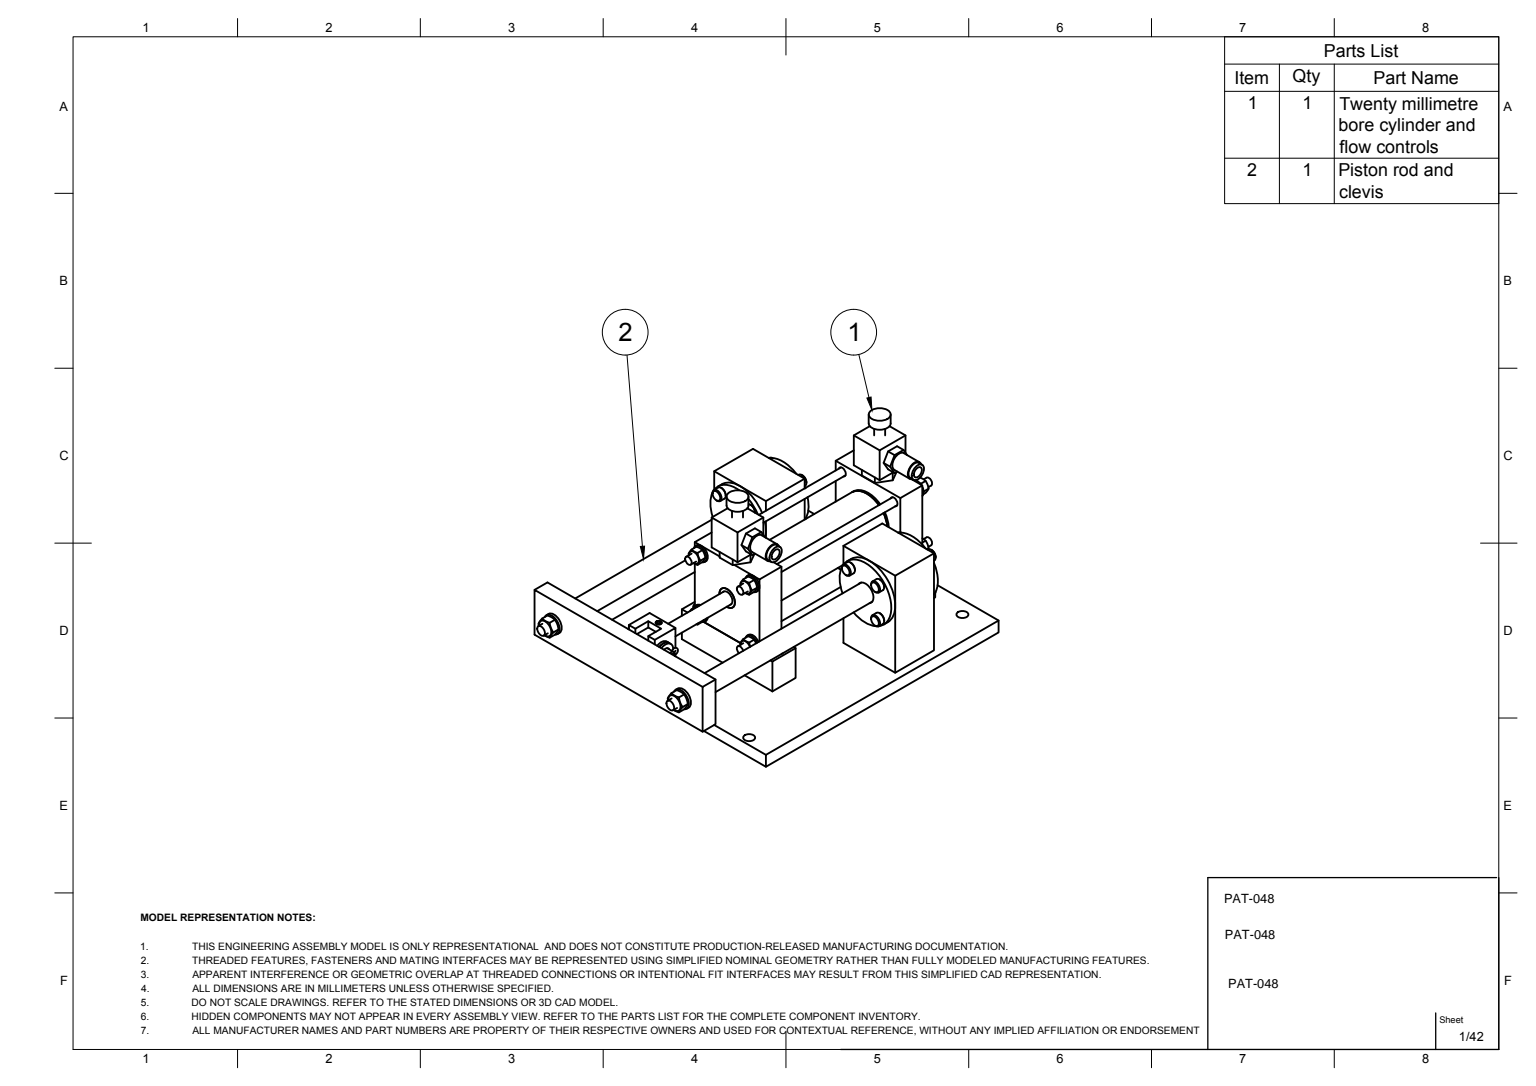
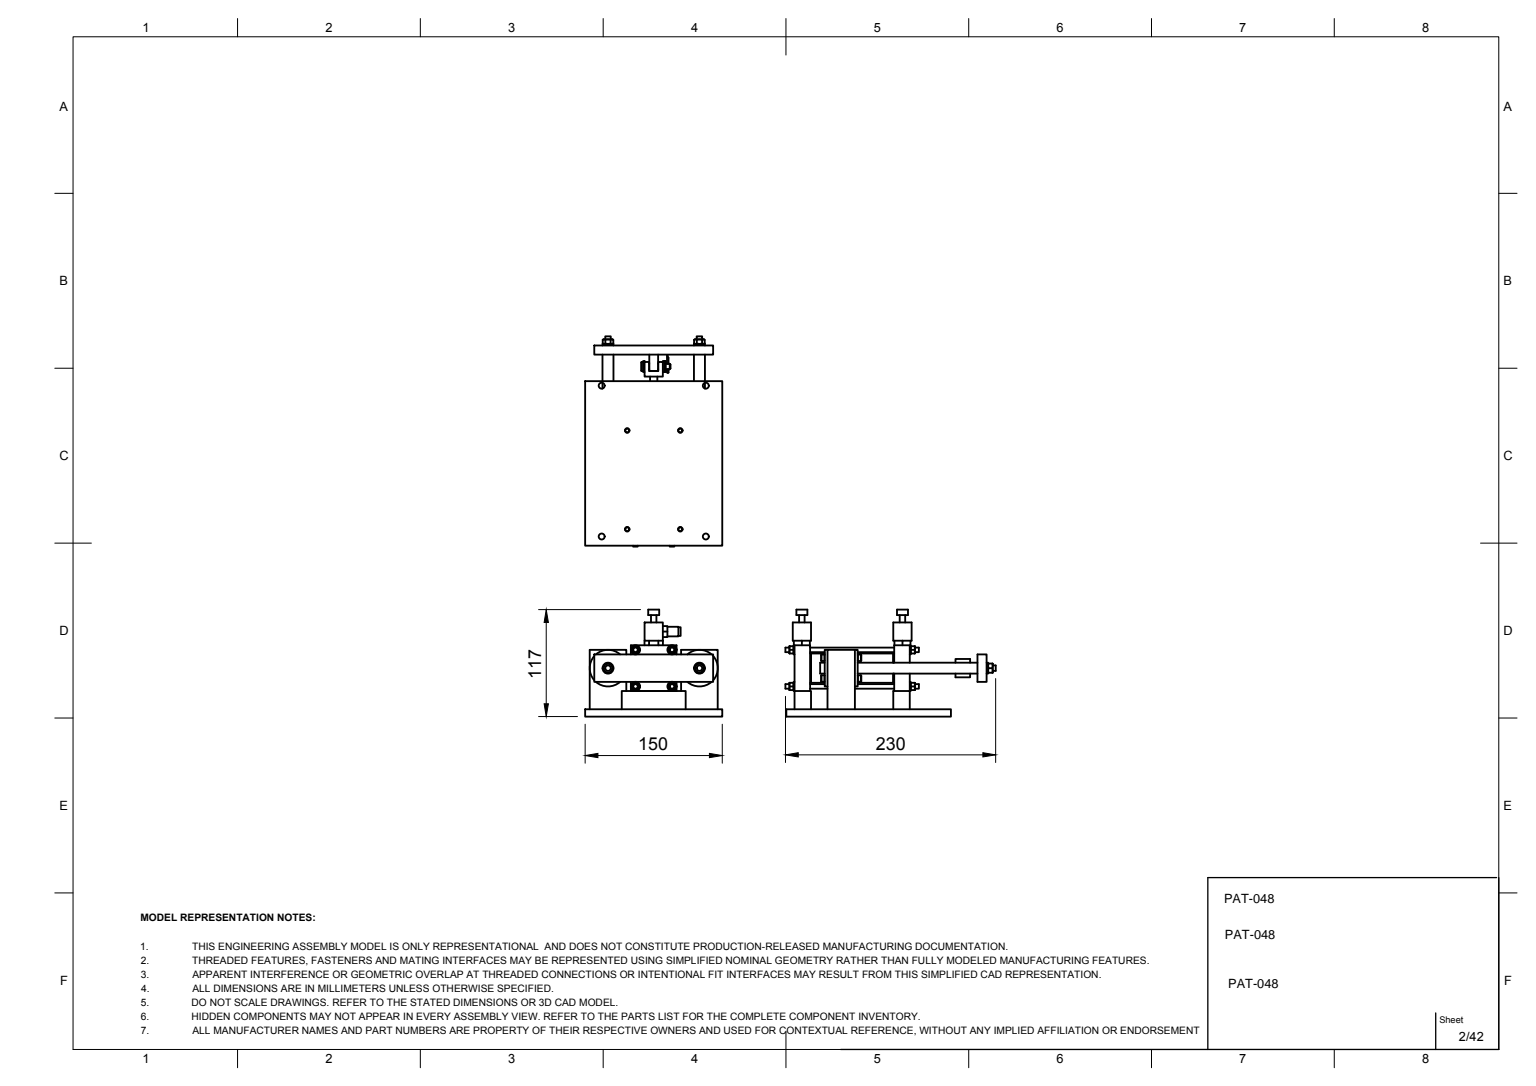
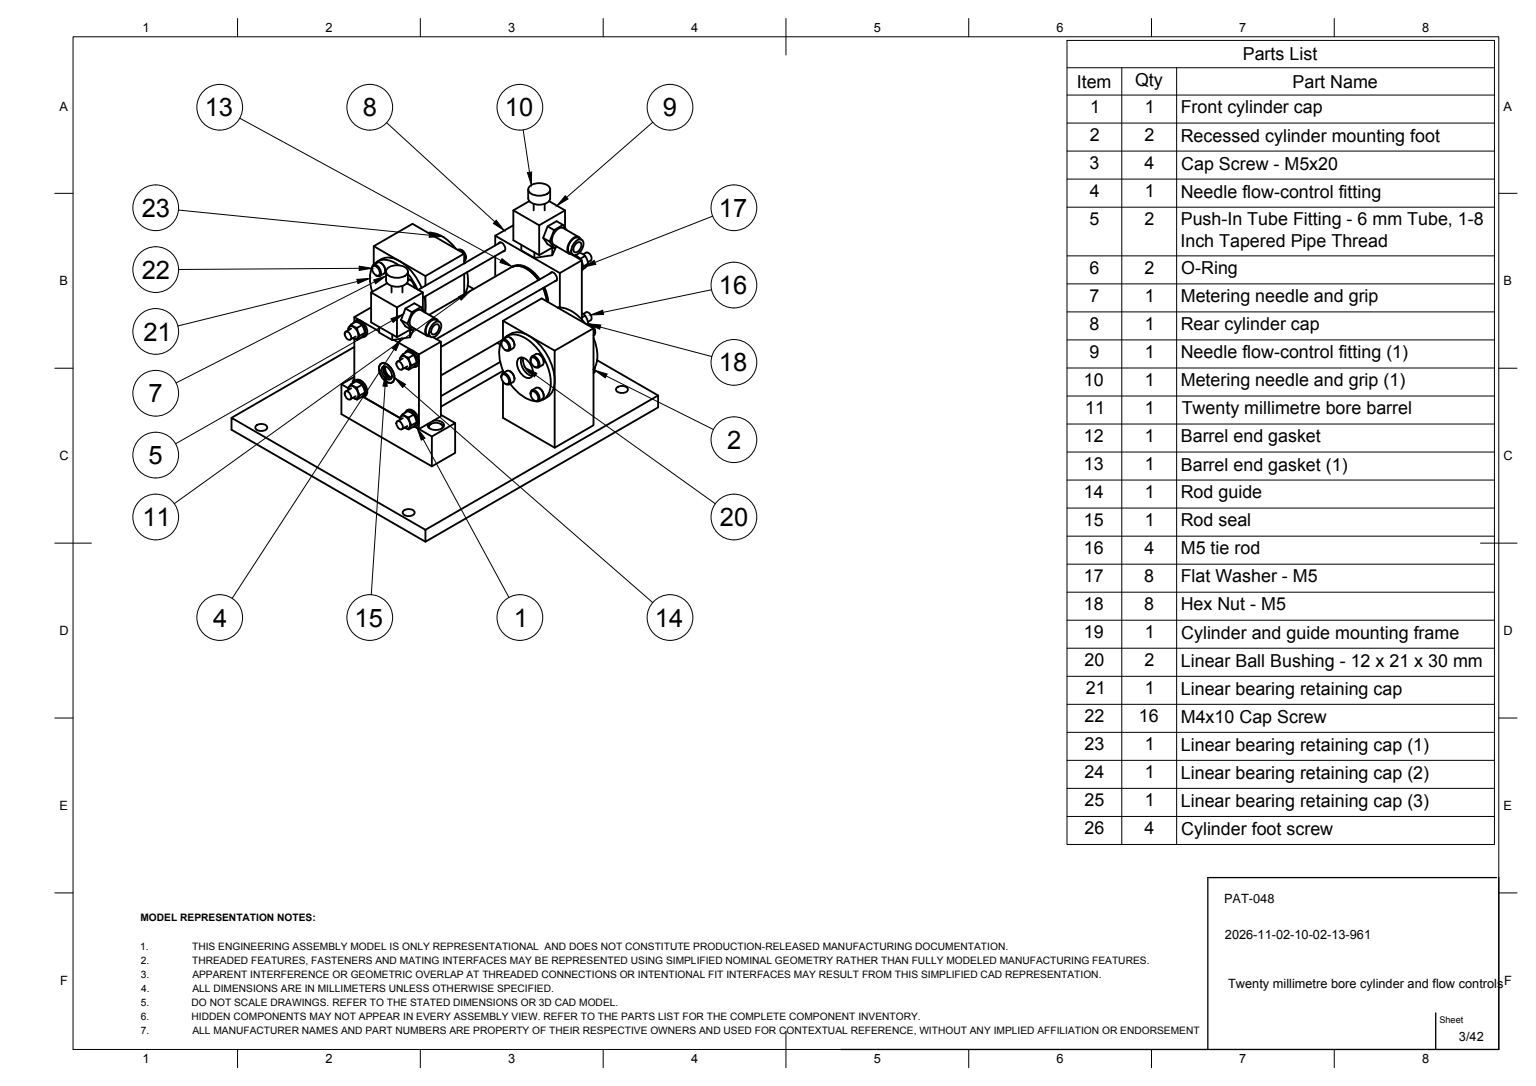
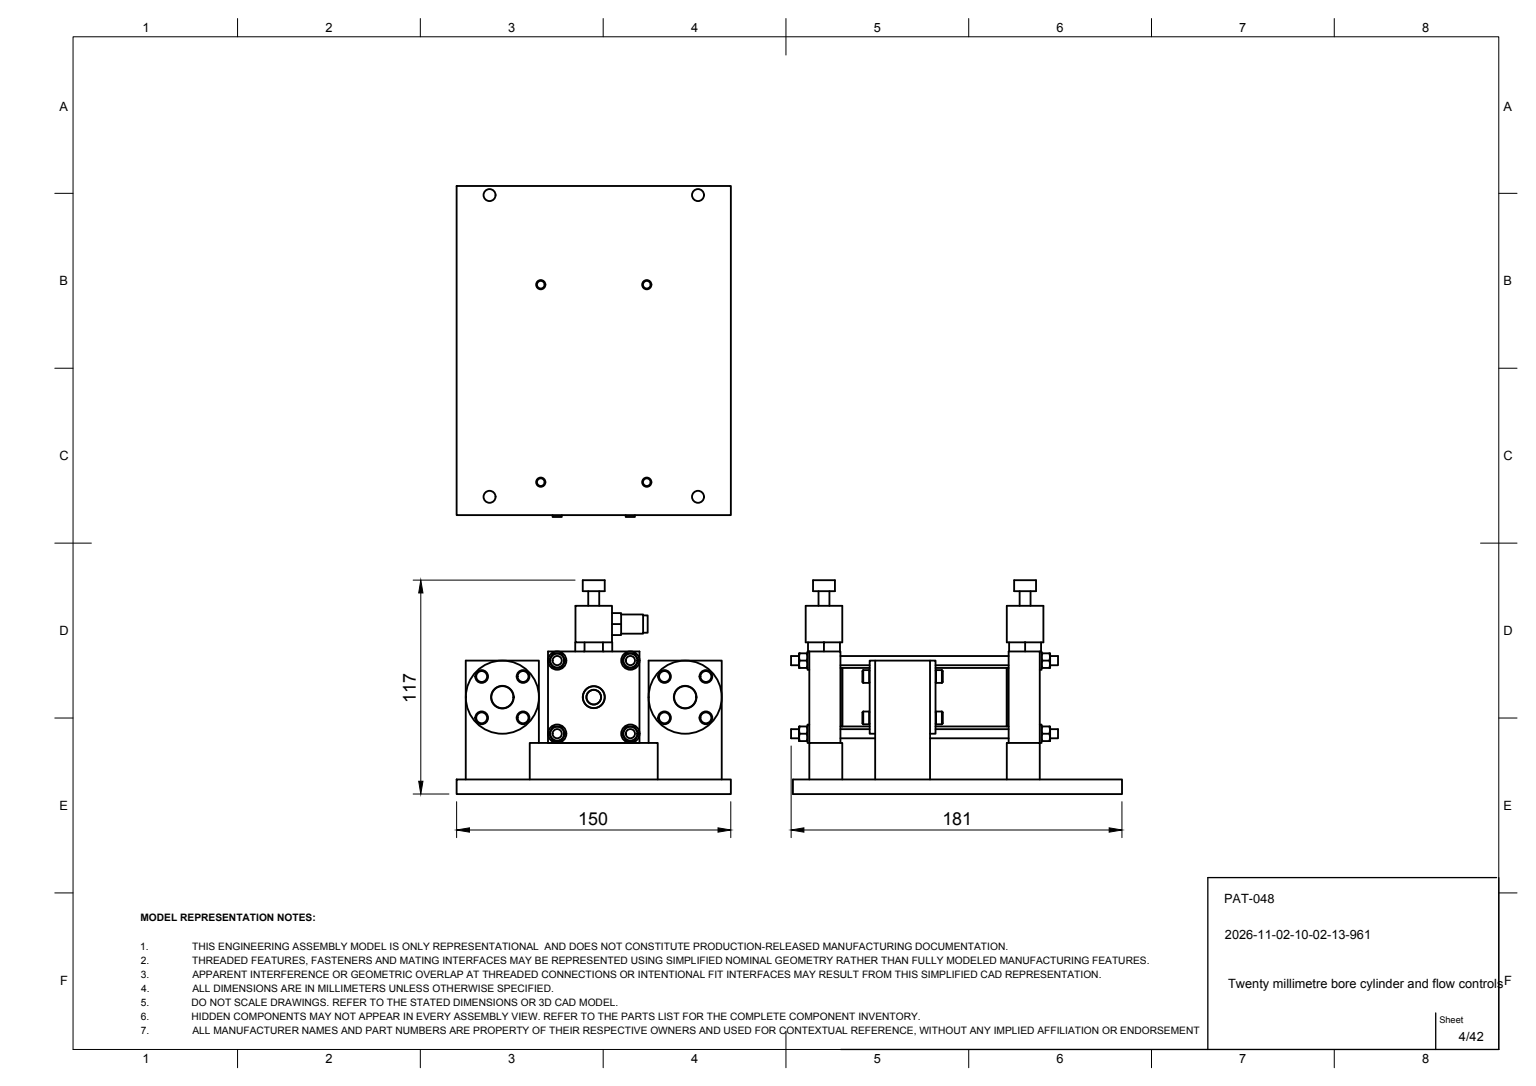
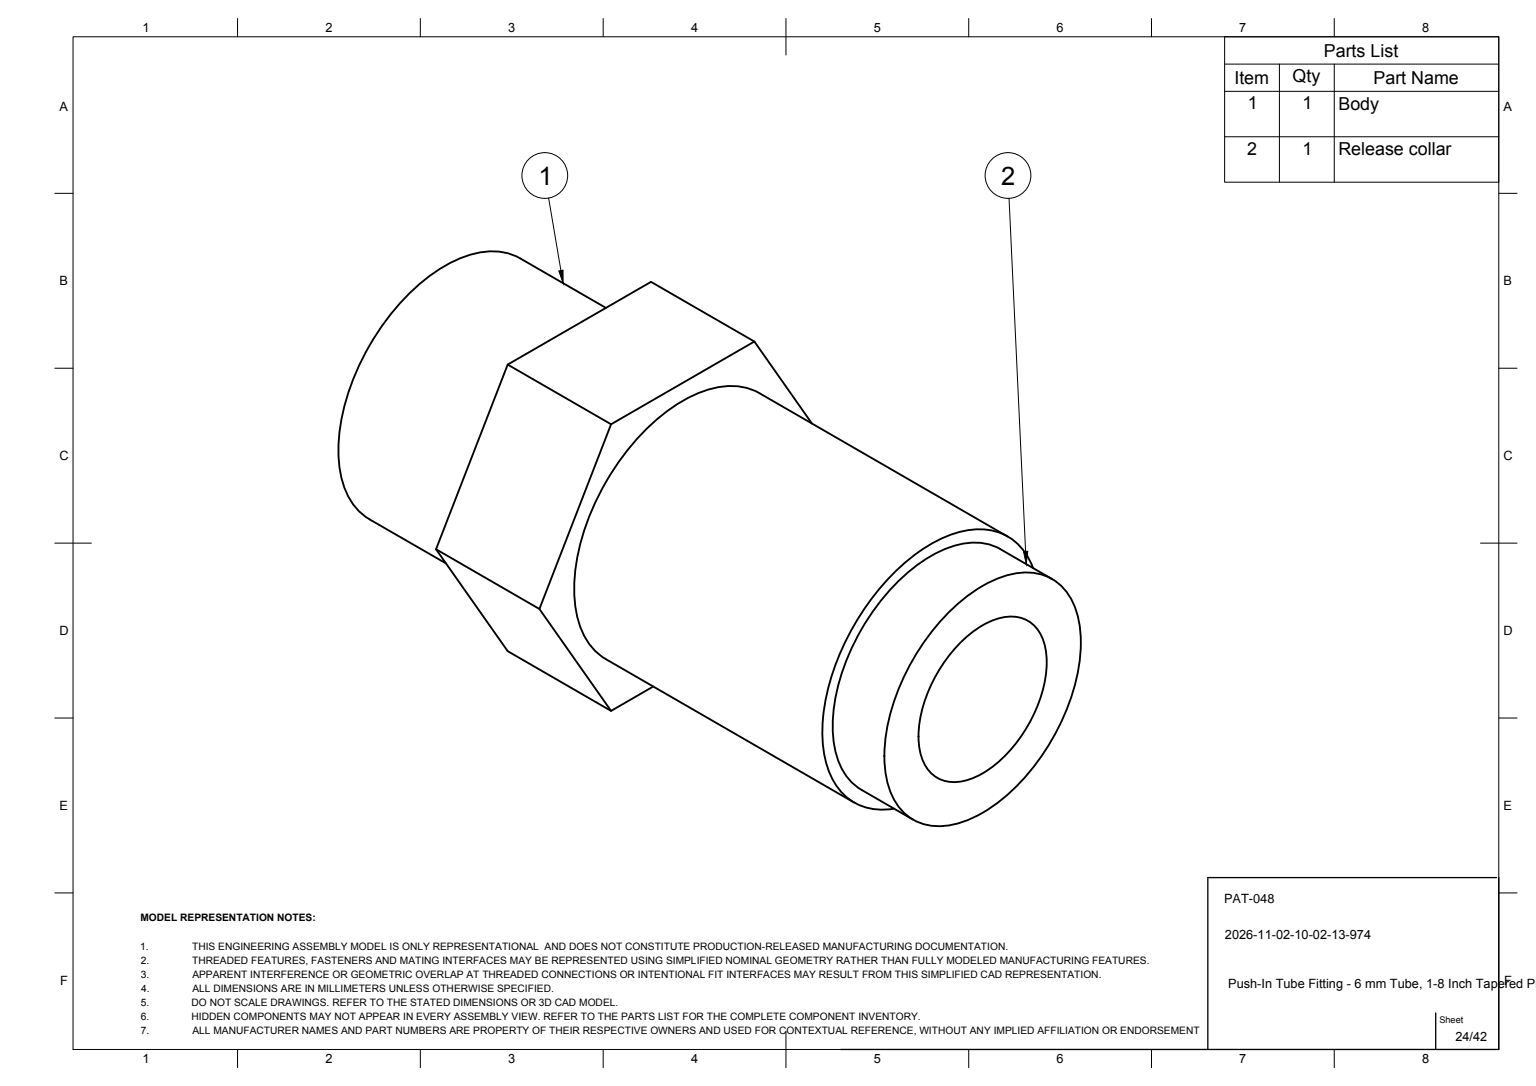
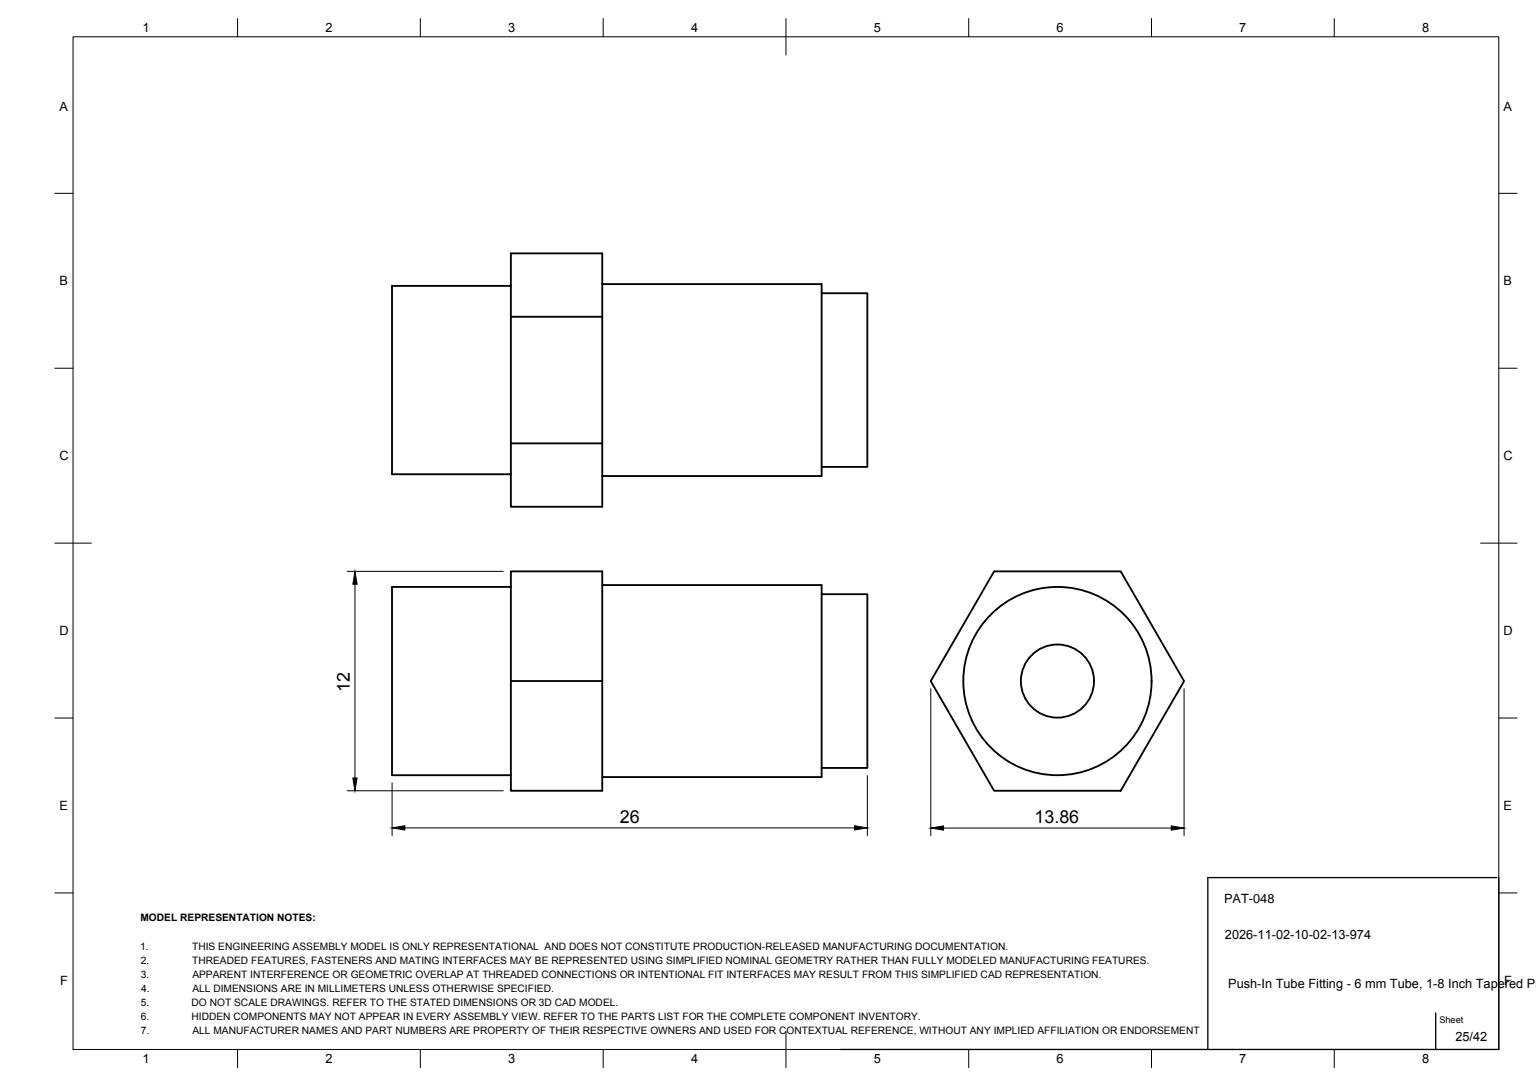
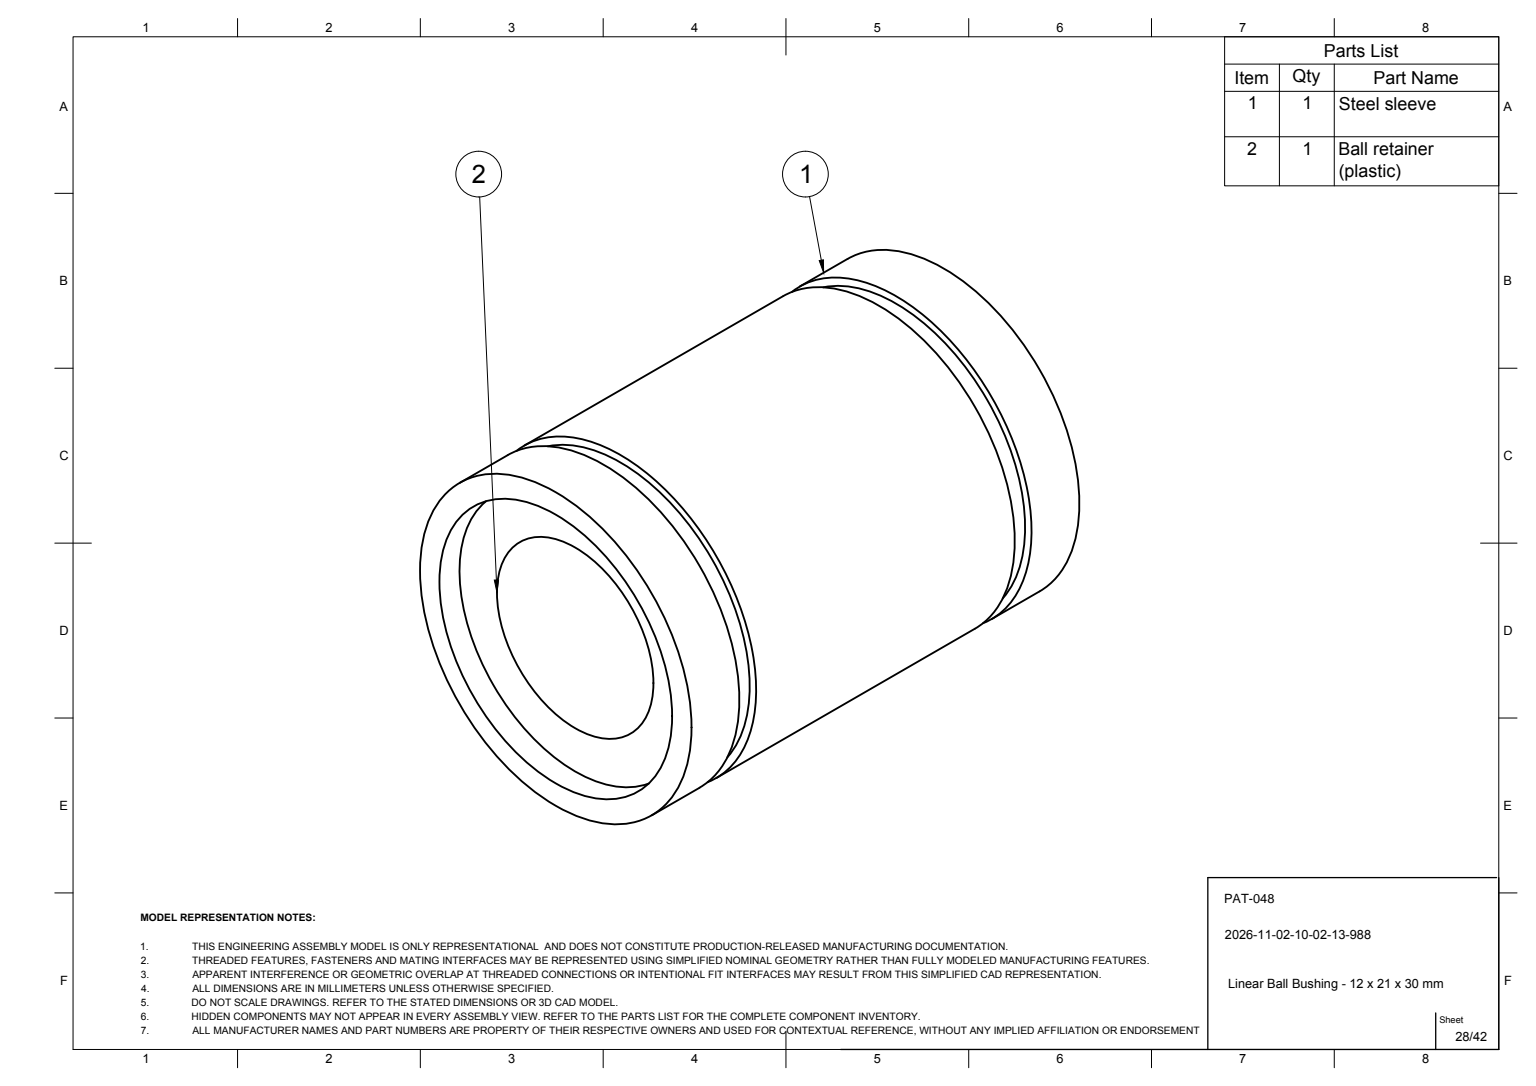
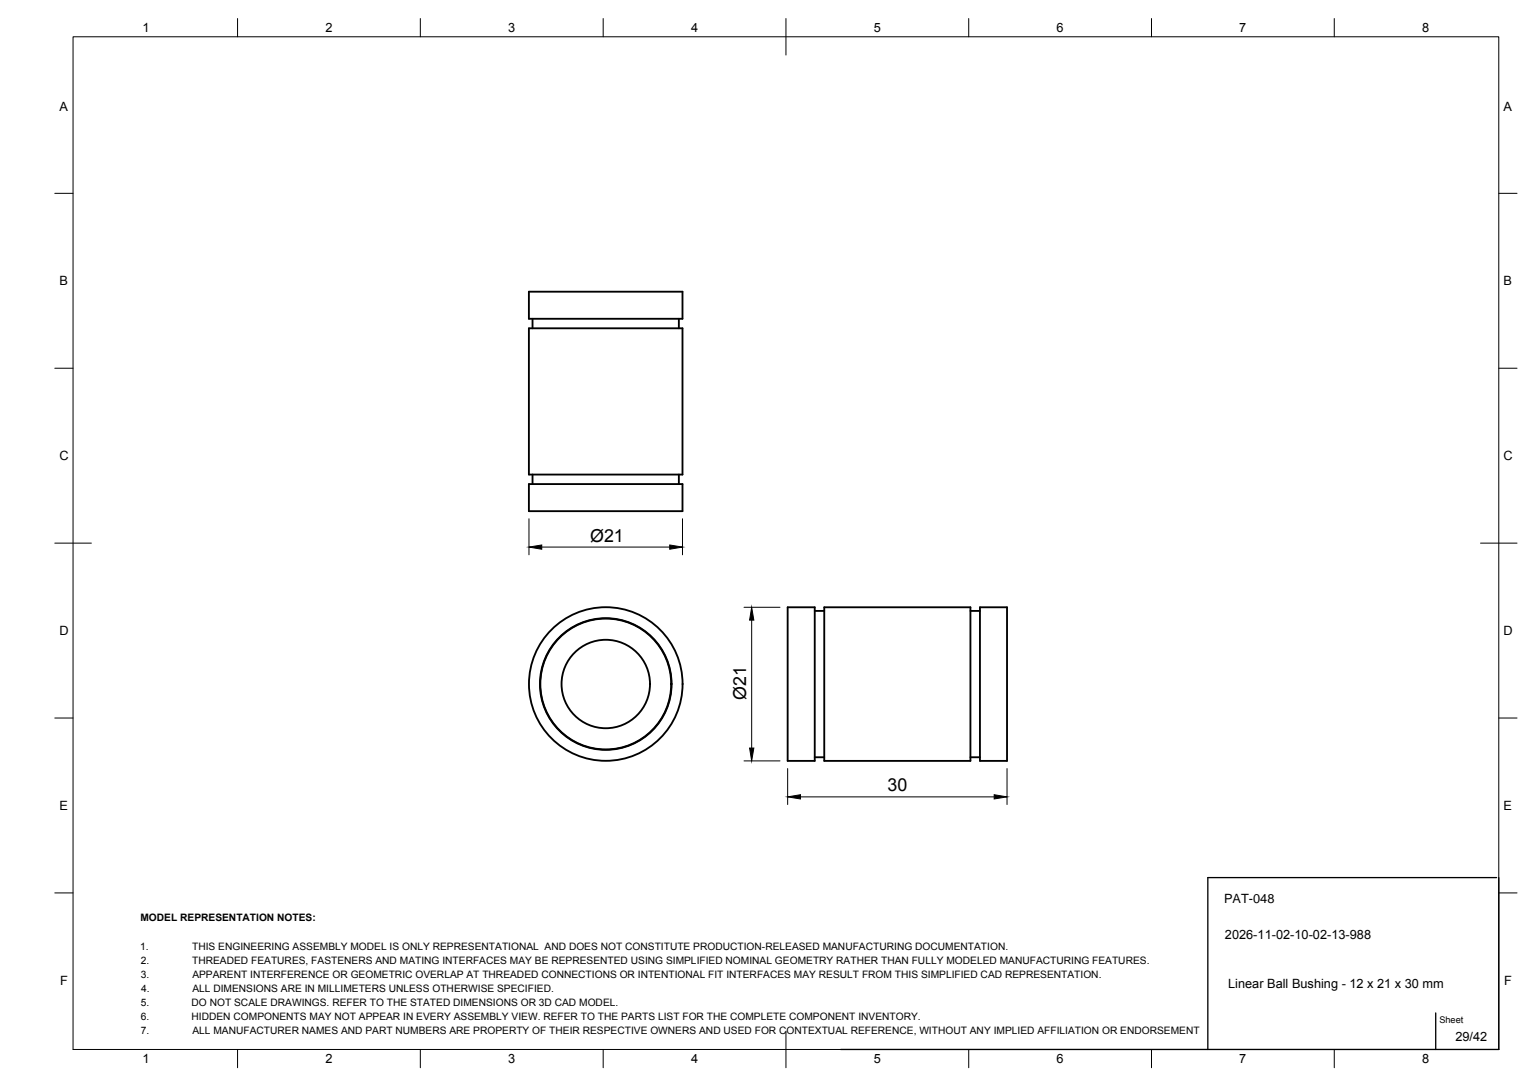
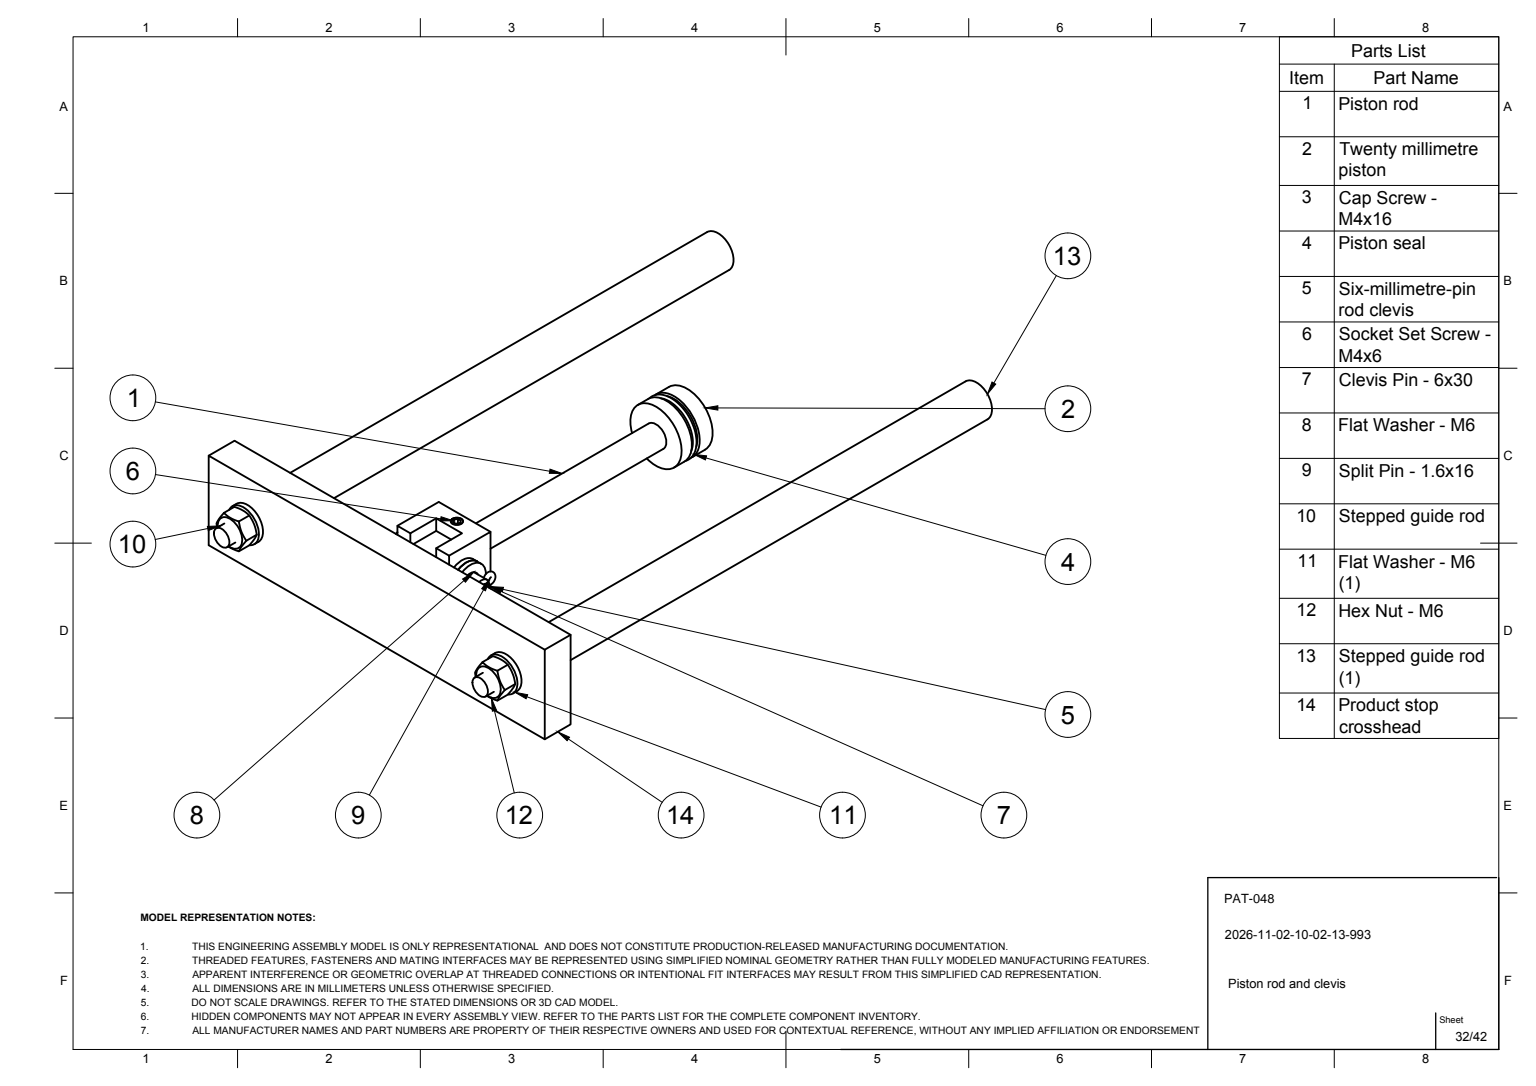
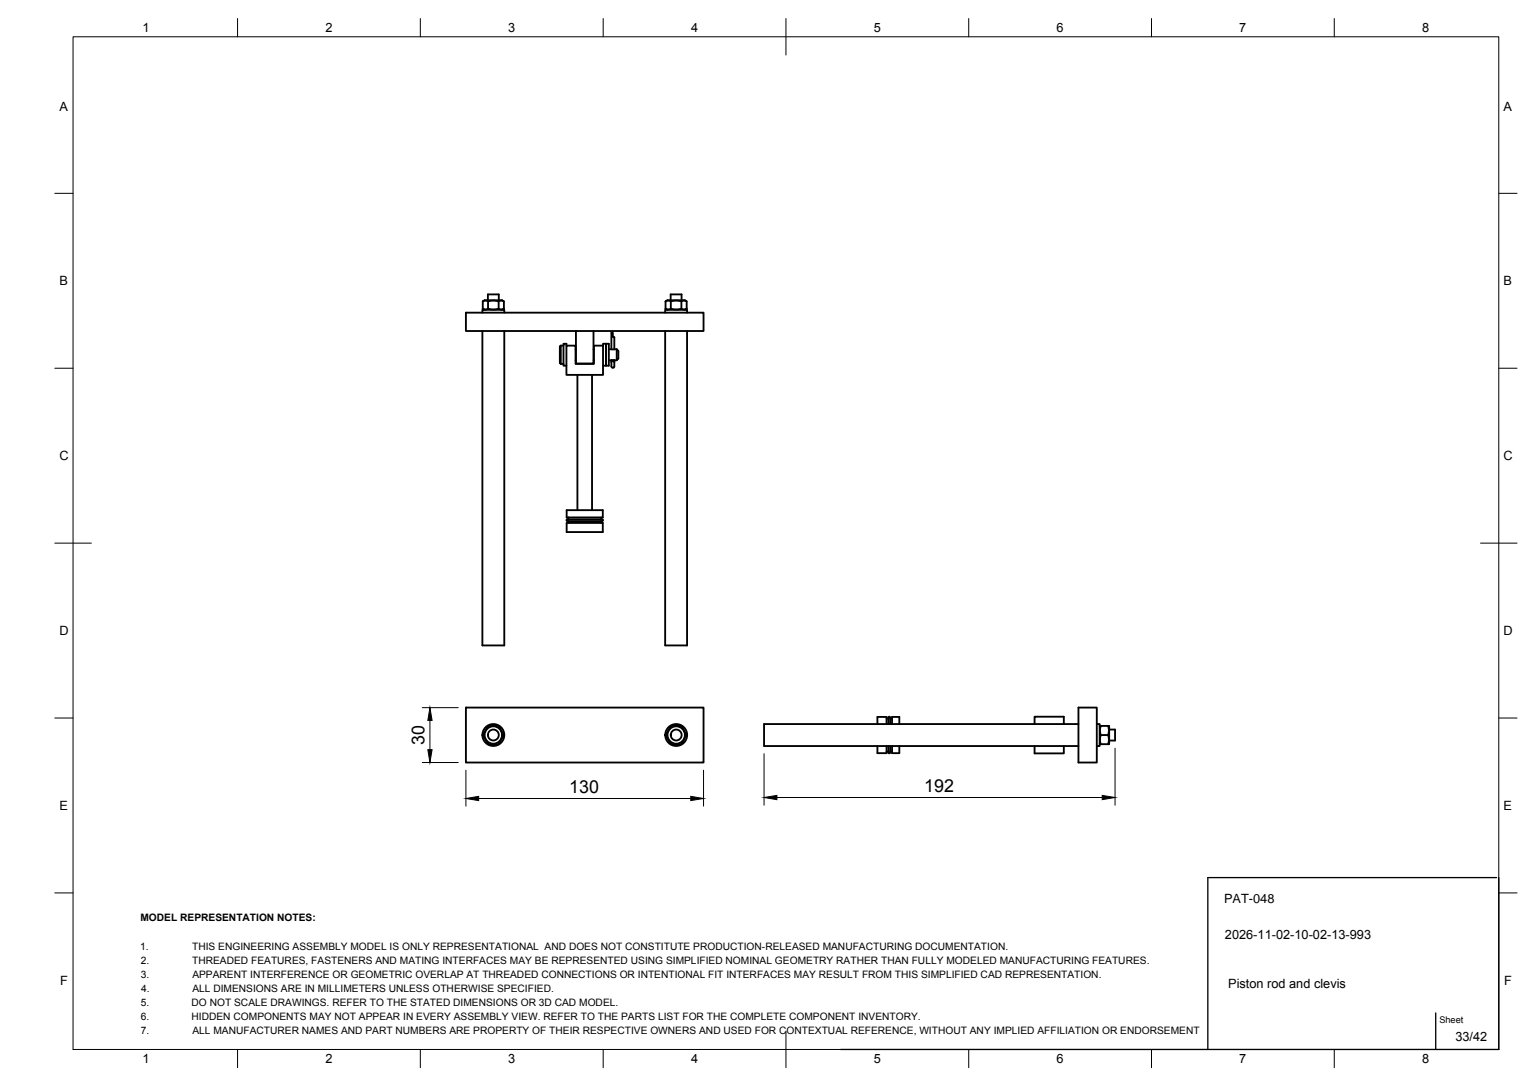
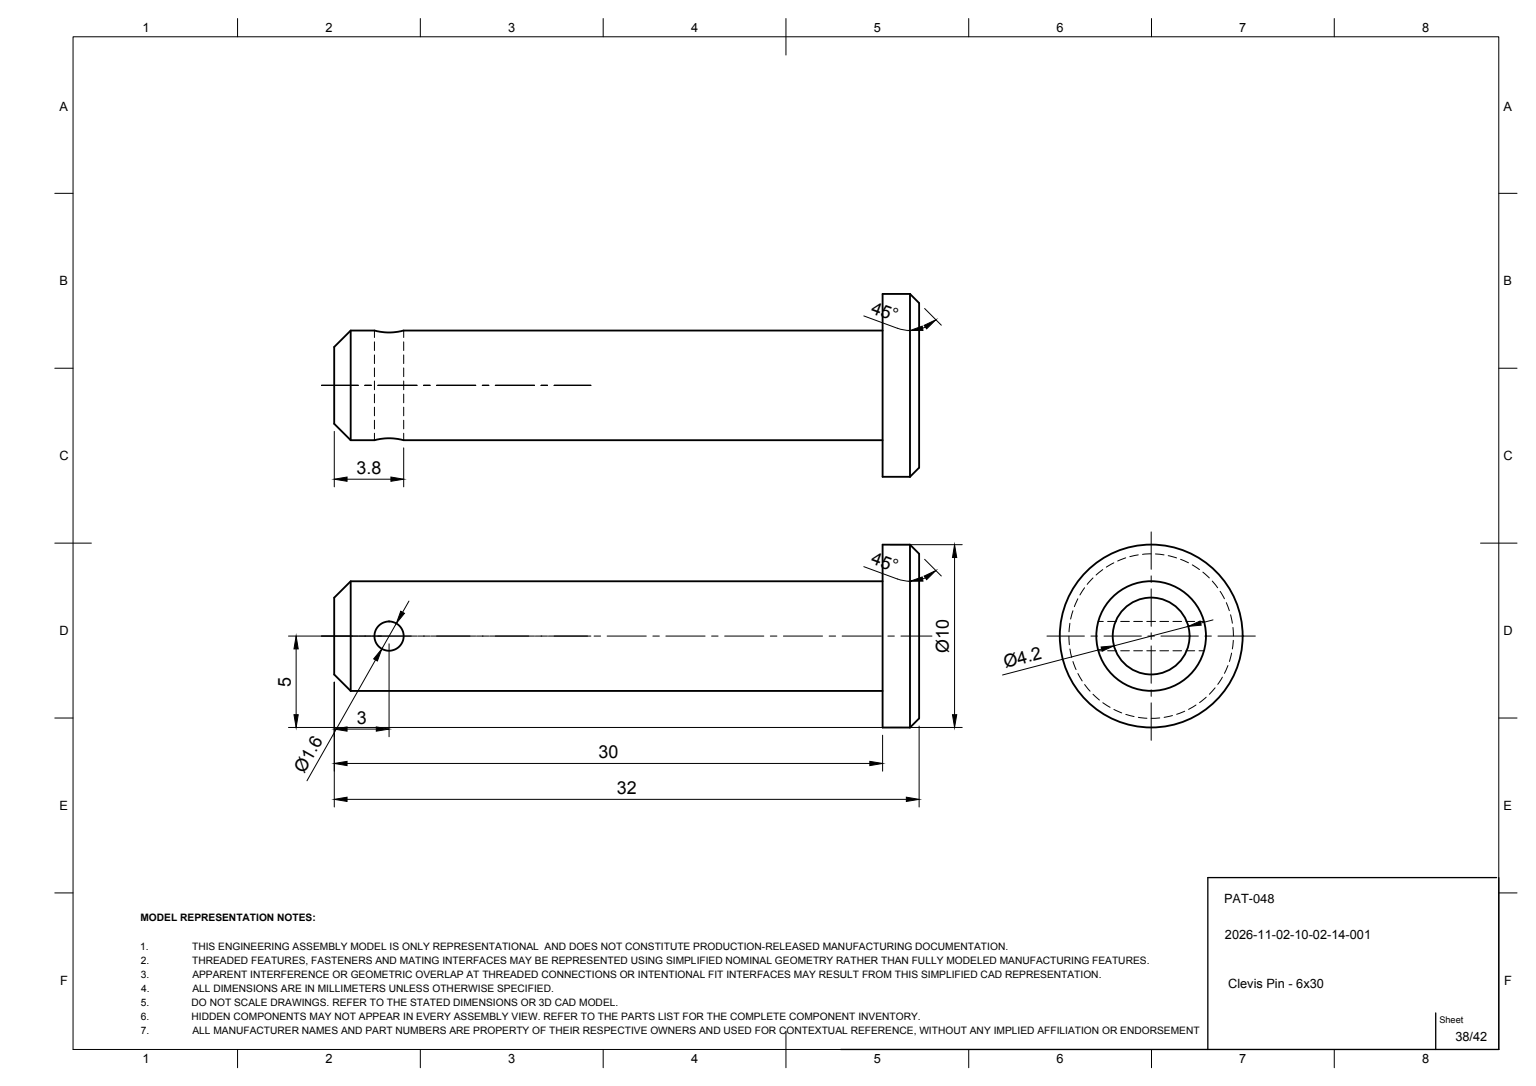
ISO-10303-21;
HEADER;
/* Generated by software containing ST-Developer
 * from STEP Tools, Inc. (www.steptools.com) 
 */

FILE_DESCRIPTION(
/* description */ ('Guided pneumatic stop gate'),
/* implementation_level */ '2;1');

FILE_NAME(
/* name */ 'PAT-048',
/* time_stamp */ '2026-10-27T21:43:45-07:00',
/* author */ (''),
/* organization */ (''),
/* preprocessor_version */ 'ST-DEVELOPER v20.2',
/* originating_system */ 'Autodesk Translation Framework v15.17.0.0',
/* authorisation */ '');

FILE_SCHEMA (('AUTOMOTIVE_DESIGN { 1 0 10303 214 3 1 1 }'));
ENDSEC;

DATA;
#10=MECHANICAL_DESIGN_GEOMETRIC_PRESENTATION_REPRESENTATION('',(#535,#536,
#537,#538,#539,#540,#541,#542,#543,#544,#545,#546,#547,#548,#549,#550,#551,
#552,#553,#554,#555,#556,#557,#558,#559,#560,#561,#562,#563,#564,#565,#566,
#567,#568,#569,#570,#571,#572,#573,#574,#575,#576),#14392);
#11=B_SPLINE_CURVE_WITH_KNOTS('',3,(#13750,#13751,#13752,#13753,#13754,
#13755,#13756,#13757,#13758,#13759),.UNSPECIFIED.,.F.,.F.,(4,2,2,2,4),(0.665271585430998,
0.692803751398643,0.75574615888762,0.818688566376597,0.846220732344242),
 .UNSPECIFIED.);
#12=B_SPLINE_CURVE_WITH_KNOTS('',3,(#13767,#13768,#13769,#13770,#13771,
#13772,#13773,#13774,#13775,#13776),.UNSPECIFIED.,.F.,.F.,(4,2,2,2,4),(0.161440812839251,
0.188972978806896,0.251915386295873,0.31485779378485,0.342389959752495),
 .UNSPECIFIED.);
#13=B_SPLINE_CURVE_WITH_KNOTS('',3,(#13893,#13894,#13895,#13896,#13897,
#13898,#13899,#13900,#13901,#13902),.UNSPECIFIED.,.F.,.F.,(4,2,2,2,4),(0.,
0.0302963256060356,0.0605926512120712,0.090883446720838,0.121174242229605),
 .UNSPECIFIED.);
#14=B_SPLINE_CURVE_WITH_KNOTS('',3,(#13905,#13906,#13907,#13908,#13909,
#13910,#13911,#13912,#13913,#13914,#13915,#13916,#13917,#13918,#13919,#13920,
#13921,#13922,#13923,#13924,#13925,#13926,#13927,#13928,#13929,#13930,#13931,
#13932,#13933,#13934,#13935,#13936,#13937,#13938),.UNSPECIFIED.,.T.,.F.,
(4,2,2,2,2,2,2,2,2,2,2,2,2,2,2,2,4),(0.,0.0302963256060358,0.0605926512120716,
0.0908834467208383,0.121174242229605,0.151465037738372,0.181755833247138,
0.212052158853174,0.24234848445921,0.272644810065246,0.302941135671282,
0.333231931180048,0.363522726688815,0.393813522197582,0.424104317706349,
0.454400643312384,0.48469696891842),.UNSPECIFIED.);
#15=B_SPLINE_CURVE_WITH_KNOTS('',3,(#13940,#13941,#13942,#13943,#13944,
#13945,#13946,#13947,#13948,#13949),.UNSPECIFIED.,.F.,.F.,(4,2,2,2,4),(0.363522726688815,
0.393813522197581,0.424104317706348,0.454400643312384,0.48469696891842),
 .UNSPECIFIED.);
#16=B_SPLINE_CURVE_WITH_KNOTS('',3,(#13950,#13951,#13952,#13953,#13954,
#13955,#13956,#13957,#13958,#13959,#13960,#13961,#13962,#13963,#13964,#13965,
#13966,#13967),.UNSPECIFIED.,.F.,.F.,(4,2,2,2,2,2,2,2,4),(0.121174242229605,
0.151465037738371,0.181755833247138,0.212052158853174,0.24234848445921,
0.272644810065246,0.302941135671281,0.333231931180048,0.363522726688815),
 .UNSPECIFIED.);
#17=B_SPLINE_CURVE_WITH_KNOTS('',3,(#14014,#14015,#14016,#14017,#14018,
#14019,#14020,#14021,#14022,#14023,#14024,#14025,#14026,#14027,#14028,#14029,
#14030,#14031,#14032,#14033,#14034,#14035,#14036,#14037,#14038,#14039),
 .UNSPECIFIED.,.F.,.F.,(4,2,2,2,2,2,2,2,2,2,2,2,4),(-0.00054581412719389,
0.,0.0281583564005144,0.0618496465371181,0.0905865724114538,0.120694112793616,
0.144966158459363,0.16923820412511,0.199345744507272,0.228082670381608,
0.261773960518212,0.289932316918681,0.290478131045882),.UNSPECIFIED.);
#18=B_SPLINE_CURVE_WITH_KNOTS('',3,(#14040,#14041,#14042,#14043,#14044,
#14045,#14046,#14047,#14048,#14049,#14050,#14051,#14052,#14053,#14054,#14055,
#14056,#14057,#14058,#14059,#14060,#14061,#14062,#14063,#14064,#14065),
 .UNSPECIFIED.,.F.,.F.,(4,2,2,2,2,2,2,2,2,2,2,2,4),(-0.000545814127196571,
0.,0.0281583564006391,0.0618496465374156,0.0905865724118984,0.120694112794215,
0.144966158460086,0.169238204125958,0.199345744508275,0.228082670382758,
0.261773960519534,0.289932316920171,0.29047813104737),.UNSPECIFIED.);
#19=(
BOUNDED_CURVE()
B_SPLINE_CURVE(2,(#12867,#12868,#12869),.UNSPECIFIED.,.F.,.F.)
B_SPLINE_CURVE_WITH_KNOTS((3,3),(0.140651836354967,0.670383167684795),
 .UNSPECIFIED.)
CURVE()
GEOMETRIC_REPRESENTATION_ITEM()
RATIONAL_B_SPLINE_CURVE((1.11602540378444,1.28867513459481,1.11602540378444))
REPRESENTATION_ITEM('')
);
#20=(
BOUNDED_CURVE()
B_SPLINE_CURVE(2,(#12871,#12872,#12873),.UNSPECIFIED.,.F.,.F.)
B_SPLINE_CURVE_WITH_KNOTS((3,3),(0.140651836354967,0.670383167684795),
 .UNSPECIFIED.)
CURVE()
GEOMETRIC_REPRESENTATION_ITEM()
RATIONAL_B_SPLINE_CURVE((1.11602540378444,1.28867513459481,1.11602540378444))
REPRESENTATION_ITEM('')
);
#21=(
BOUNDED_CURVE()
B_SPLINE_CURVE(2,(#12878,#12879,#12880),.UNSPECIFIED.,.F.,.F.)
B_SPLINE_CURVE_WITH_KNOTS((3,3),(0.140651836354967,0.670383167684795),
 .UNSPECIFIED.)
CURVE()
GEOMETRIC_REPRESENTATION_ITEM()
RATIONAL_B_SPLINE_CURVE((1.11602540378444,1.28867513459481,1.11602540378444))
REPRESENTATION_ITEM('')
);
#22=(
BOUNDED_CURVE()
B_SPLINE_CURVE(2,(#12882,#12883,#12884),.UNSPECIFIED.,.F.,.F.)
B_SPLINE_CURVE_WITH_KNOTS((3,3),(0.140651836354967,0.670383167684795),
 .UNSPECIFIED.)
CURVE()
GEOMETRIC_REPRESENTATION_ITEM()
RATIONAL_B_SPLINE_CURVE((1.11602540378444,1.28867513459481,1.11602540378444))
REPRESENTATION_ITEM('')
);
#23=(
BOUNDED_CURVE()
B_SPLINE_CURVE(2,(#12886,#12887,#12888),.UNSPECIFIED.,.F.,.F.)
B_SPLINE_CURVE_WITH_KNOTS((3,3),(0.140651836354967,0.670383167684795),
 .UNSPECIFIED.)
CURVE()
GEOMETRIC_REPRESENTATION_ITEM()
RATIONAL_B_SPLINE_CURVE((1.11602540378444,1.28867513459481,1.11602540378444))
REPRESENTATION_ITEM('')
);
#24=(
BOUNDED_CURVE()
B_SPLINE_CURVE(2,(#12889,#12890,#12891),.UNSPECIFIED.,.F.,.F.)
B_SPLINE_CURVE_WITH_KNOTS((3,3),(0.140651836354967,0.670383167684795),
 .UNSPECIFIED.)
CURVE()
GEOMETRIC_REPRESENTATION_ITEM()
RATIONAL_B_SPLINE_CURVE((1.11602540378444,1.28867513459481,1.11602540378444))
REPRESENTATION_ITEM('')
);
#25=(
BOUNDED_CURVE()
B_SPLINE_CURVE(2,(#12898,#12899,#12900),.UNSPECIFIED.,.F.,.F.)
B_SPLINE_CURVE_WITH_KNOTS((3,3),(0.140651836354967,0.670383167684795),
 .UNSPECIFIED.)
CURVE()
GEOMETRIC_REPRESENTATION_ITEM()
RATIONAL_B_SPLINE_CURVE((1.11602540378444,1.28867513459481,1.11602540378444))
REPRESENTATION_ITEM('')
);
#26=(
BOUNDED_CURVE()
B_SPLINE_CURVE(2,(#12902,#12903,#12904),.UNSPECIFIED.,.F.,.F.)
B_SPLINE_CURVE_WITH_KNOTS((3,3),(0.140651836354967,0.670383167684796),
 .UNSPECIFIED.)
CURVE()
GEOMETRIC_REPRESENTATION_ITEM()
RATIONAL_B_SPLINE_CURVE((1.11602540378444,1.28867513459481,1.11602540378444))
REPRESENTATION_ITEM('')
);
#27=(
BOUNDED_CURVE()
B_SPLINE_CURVE(2,(#12906,#12907,#12908),.UNSPECIFIED.,.F.,.F.)
B_SPLINE_CURVE_WITH_KNOTS((3,3),(0.140651836354967,0.670383167684795),
 .UNSPECIFIED.)
CURVE()
GEOMETRIC_REPRESENTATION_ITEM()
RATIONAL_B_SPLINE_CURVE((1.11602540378444,1.28867513459481,1.11602540378444))
REPRESENTATION_ITEM('')
);
#28=(
BOUNDED_CURVE()
B_SPLINE_CURVE(2,(#12910,#12911,#12912),.UNSPECIFIED.,.F.,.F.)
B_SPLINE_CURVE_WITH_KNOTS((3,3),(0.140651836354967,0.670383167684795),
 .UNSPECIFIED.)
CURVE()
GEOMETRIC_REPRESENTATION_ITEM()
RATIONAL_B_SPLINE_CURVE((1.11602540378444,1.28867513459482,1.11602540378444))
REPRESENTATION_ITEM('')
);
#29=(
BOUNDED_CURVE()
B_SPLINE_CURVE(2,(#12914,#12915,#12916),.UNSPECIFIED.,.F.,.F.)
B_SPLINE_CURVE_WITH_KNOTS((3,3),(0.140651836354967,0.670383167684795),
 .UNSPECIFIED.)
CURVE()
GEOMETRIC_REPRESENTATION_ITEM()
RATIONAL_B_SPLINE_CURVE((1.11602540378444,1.28867513459481,1.11602540378444))
REPRESENTATION_ITEM('')
);
#30=(
BOUNDED_CURVE()
B_SPLINE_CURVE(2,(#12917,#12918,#12919),.UNSPECIFIED.,.F.,.F.)
B_SPLINE_CURVE_WITH_KNOTS((3,3),(0.140651836354967,0.670383167684795),
 .UNSPECIFIED.)
CURVE()
GEOMETRIC_REPRESENTATION_ITEM()
RATIONAL_B_SPLINE_CURVE((1.11602540378444,1.28867513459481,1.11602540378444))
REPRESENTATION_ITEM('')
);
#31=(
BOUNDED_CURVE()
B_SPLINE_CURVE(2,(#14204,#14205,#14206),.UNSPECIFIED.,.F.,.F.)
B_SPLINE_CURVE_WITH_KNOTS((3,3),(0.144988513094728,0.791574906712449),
 .UNSPECIFIED.)
CURVE()
GEOMETRIC_REPRESENTATION_ITEM()
RATIONAL_B_SPLINE_CURVE((1.09282032302755,1.26188021535082,1.09282032302931))
REPRESENTATION_ITEM('')
);
#32=(
BOUNDED_CURVE()
B_SPLINE_CURVE(2,(#14208,#14209,#14210),.UNSPECIFIED.,.F.,.F.)
B_SPLINE_CURVE_WITH_KNOTS((3,3),(0.144988513094728,0.791574906712449),
 .UNSPECIFIED.)
CURVE()
GEOMETRIC_REPRESENTATION_ITEM()
RATIONAL_B_SPLINE_CURVE((1.09282032302755,1.26188021535082,1.09282032302931))
REPRESENTATION_ITEM('')
);
#33=(
BOUNDED_CURVE()
B_SPLINE_CURVE(2,(#14215,#14216,#14217),.UNSPECIFIED.,.F.,.F.)
B_SPLINE_CURVE_WITH_KNOTS((3,3),(0.144988513094728,0.791574906712449),
 .UNSPECIFIED.)
CURVE()
GEOMETRIC_REPRESENTATION_ITEM()
RATIONAL_B_SPLINE_CURVE((1.09282032302755,1.26188021535082,1.09282032302931))
REPRESENTATION_ITEM('')
);
#34=(
BOUNDED_CURVE()
B_SPLINE_CURVE(2,(#14219,#14220,#14221),.UNSPECIFIED.,.F.,.F.)
B_SPLINE_CURVE_WITH_KNOTS((3,3),(0.144988513094728,0.791574906712449),
 .UNSPECIFIED.)
CURVE()
GEOMETRIC_REPRESENTATION_ITEM()
RATIONAL_B_SPLINE_CURVE((1.09282032302755,1.26188021535082,1.09282032302931))
REPRESENTATION_ITEM('')
);
#35=(
BOUNDED_CURVE()
B_SPLINE_CURVE(2,(#14223,#14224,#14225),.UNSPECIFIED.,.F.,.F.)
B_SPLINE_CURVE_WITH_KNOTS((3,3),(0.144988513094728,0.791574906712449),
 .UNSPECIFIED.)
CURVE()
GEOMETRIC_REPRESENTATION_ITEM()
RATIONAL_B_SPLINE_CURVE((1.09282032302755,1.26188021535082,1.09282032302931))
REPRESENTATION_ITEM('')
);
#36=(
BOUNDED_CURVE()
B_SPLINE_CURVE(2,(#14226,#14227,#14228),.UNSPECIFIED.,.F.,.F.)
B_SPLINE_CURVE_WITH_KNOTS((3,3),(0.144988513094728,0.791574906712449),
 .UNSPECIFIED.)
CURVE()
GEOMETRIC_REPRESENTATION_ITEM()
RATIONAL_B_SPLINE_CURVE((1.09282032302755,1.26188021535082,1.09282032302931))
REPRESENTATION_ITEM('')
);
#37=(
BOUNDED_CURVE()
B_SPLINE_CURVE(2,(#14235,#14236,#14237),.UNSPECIFIED.,.F.,.F.)
B_SPLINE_CURVE_WITH_KNOTS((3,3),(0.144988513094728,0.791574906712449),
 .UNSPECIFIED.)
CURVE()
GEOMETRIC_REPRESENTATION_ITEM()
RATIONAL_B_SPLINE_CURVE((1.09282032302755,1.26188021535082,1.09282032302931))
REPRESENTATION_ITEM('')
);
#38=(
BOUNDED_CURVE()
B_SPLINE_CURVE(2,(#14239,#14240,#14241),.UNSPECIFIED.,.F.,.F.)
B_SPLINE_CURVE_WITH_KNOTS((3,3),(0.144988513094727,0.791574906712449),
 .UNSPECIFIED.)
CURVE()
GEOMETRIC_REPRESENTATION_ITEM()
RATIONAL_B_SPLINE_CURVE((1.09282032302755,1.26188021535082,1.09282032302931))
REPRESENTATION_ITEM('')
);
#39=(
BOUNDED_CURVE()
B_SPLINE_CURVE(2,(#14243,#14244,#14245),.UNSPECIFIED.,.F.,.F.)
B_SPLINE_CURVE_WITH_KNOTS((3,3),(0.144988513094728,0.791574906712449),
 .UNSPECIFIED.)
CURVE()
GEOMETRIC_REPRESENTATION_ITEM()
RATIONAL_B_SPLINE_CURVE((1.09282032302755,1.26188021535082,1.09282032302931))
REPRESENTATION_ITEM('')
);
#40=(
BOUNDED_CURVE()
B_SPLINE_CURVE(2,(#14247,#14248,#14249),.UNSPECIFIED.,.F.,.F.)
B_SPLINE_CURVE_WITH_KNOTS((3,3),(0.144988513094728,0.791574906712449),
 .UNSPECIFIED.)
CURVE()
GEOMETRIC_REPRESENTATION_ITEM()
RATIONAL_B_SPLINE_CURVE((1.09282032302755,1.26188021535082,1.09282032302931))
REPRESENTATION_ITEM('')
);
#41=(
BOUNDED_CURVE()
B_SPLINE_CURVE(2,(#14251,#14252,#14253),.UNSPECIFIED.,.F.,.F.)
B_SPLINE_CURVE_WITH_KNOTS((3,3),(0.144988513094728,0.791574906712449),
 .UNSPECIFIED.)
CURVE()
GEOMETRIC_REPRESENTATION_ITEM()
RATIONAL_B_SPLINE_CURVE((1.09282032302755,1.26188021535082,1.09282032302931))
REPRESENTATION_ITEM('')
);
#42=(
BOUNDED_CURVE()
B_SPLINE_CURVE(2,(#14254,#14255,#14256),.UNSPECIFIED.,.F.,.F.)
B_SPLINE_CURVE_WITH_KNOTS((3,3),(0.144988513094727,0.791574906712449),
 .UNSPECIFIED.)
CURVE()
GEOMETRIC_REPRESENTATION_ITEM()
RATIONAL_B_SPLINE_CURVE((1.09282032302755,1.26188021535082,1.09282032302931))
REPRESENTATION_ITEM('')
);
#43=TOROIDAL_SURFACE('',#8768,0.3925,0.089);
#44=TOROIDAL_SURFACE('',#8789,0.45,0.05);
#45=TOROIDAL_SURFACE('',#9177,0.95,0.05);
#46=TOROIDAL_SURFACE('',#9285,0.12,0.08);
#47=ITEM_DEFINED_TRANSFORMATION($,$,#8724,#8765);
#48=ITEM_DEFINED_TRANSFORMATION($,$,#8752,#8766);
#49=ITEM_DEFINED_TRANSFORMATION($,$,#8981,#9030);
#50=ITEM_DEFINED_TRANSFORMATION($,$,#9013,#9031);
#51=ITEM_DEFINED_TRANSFORMATION($,$,#8386,#9086);
#52=ITEM_DEFINED_TRANSFORMATION($,$,#8456,#9087);
#53=ITEM_DEFINED_TRANSFORMATION($,$,#8500,#9088);
#54=ITEM_DEFINED_TRANSFORMATION($,$,#8512,#9089);
#55=ITEM_DEFINED_TRANSFORMATION($,$,#8579,#9090);
#56=ITEM_DEFINED_TRANSFORMATION($,$,#8623,#9091);
#57=ITEM_DEFINED_TRANSFORMATION($,$,#8635,#9092);
#58=ITEM_DEFINED_TRANSFORMATION($,$,#8644,#9093);
#59=ITEM_DEFINED_TRANSFORMATION($,$,#8653,#9094);
#60=ITEM_DEFINED_TRANSFORMATION($,$,#8662,#9095);
#61=ITEM_DEFINED_TRANSFORMATION($,$,#8697,#9096);
#62=ITEM_DEFINED_TRANSFORMATION($,$,#8697,#9097);
#63=ITEM_DEFINED_TRANSFORMATION($,$,#8723,#9098);
#64=ITEM_DEFINED_TRANSFORMATION($,$,#8767,#9099);
#65=ITEM_DEFINED_TRANSFORMATION($,$,#8662,#9100);
#66=ITEM_DEFINED_TRANSFORMATION($,$,#8697,#9101);
#67=ITEM_DEFINED_TRANSFORMATION($,$,#8697,#9102);
#68=ITEM_DEFINED_TRANSFORMATION($,$,#8723,#9103);
#69=ITEM_DEFINED_TRANSFORMATION($,$,#8767,#9104);
#70=ITEM_DEFINED_TRANSFORMATION($,$,#8771,#9105);
#71=ITEM_DEFINED_TRANSFORMATION($,$,#8788,#9106);
#72=ITEM_DEFINED_TRANSFORMATION($,$,#8792,#9107);
#73=ITEM_DEFINED_TRANSFORMATION($,$,#8798,#9108);
#74=ITEM_DEFINED_TRANSFORMATION($,$,#8809,#9109);
#75=ITEM_DEFINED_TRANSFORMATION($,$,#8798,#9110);
#76=ITEM_DEFINED_TRANSFORMATION($,$,#8809,#9111);
#77=ITEM_DEFINED_TRANSFORMATION($,$,#8792,#9112);
#78=ITEM_DEFINED_TRANSFORMATION($,$,#8798,#9113);
#79=ITEM_DEFINED_TRANSFORMATION($,$,#8809,#9114);
#80=ITEM_DEFINED_TRANSFORMATION($,$,#8798,#9115);
#81=ITEM_DEFINED_TRANSFORMATION($,$,#8809,#9116);
#82=ITEM_DEFINED_TRANSFORMATION($,$,#8792,#9117);
#83=ITEM_DEFINED_TRANSFORMATION($,$,#8798,#9118);
#84=ITEM_DEFINED_TRANSFORMATION($,$,#8809,#9119);
#85=ITEM_DEFINED_TRANSFORMATION($,$,#8798,#9120);
#86=ITEM_DEFINED_TRANSFORMATION($,$,#8809,#9121);
#87=ITEM_DEFINED_TRANSFORMATION($,$,#8792,#9122);
#88=ITEM_DEFINED_TRANSFORMATION($,$,#8798,#9123);
#89=ITEM_DEFINED_TRANSFORMATION($,$,#8809,#9124);
#90=ITEM_DEFINED_TRANSFORMATION($,$,#8798,#9125);
#91=ITEM_DEFINED_TRANSFORMATION($,$,#8809,#9126);
#92=ITEM_DEFINED_TRANSFORMATION($,$,#8825,#9127);
#93=ITEM_DEFINED_TRANSFORMATION($,$,#8896,#9128);
#94=ITEM_DEFINED_TRANSFORMATION($,$,#8917,#9129);
#95=ITEM_DEFINED_TRANSFORMATION($,$,#8938,#9130);
#96=ITEM_DEFINED_TRANSFORMATION($,$,#8959,#9131);
#97=ITEM_DEFINED_TRANSFORMATION($,$,#8980,#9132);
#98=ITEM_DEFINED_TRANSFORMATION($,$,#9032,#9133);
#99=ITEM_DEFINED_TRANSFORMATION($,$,#9032,#9134);
#100=ITEM_DEFINED_TRANSFORMATION($,$,#9032,#9135);
#101=ITEM_DEFINED_TRANSFORMATION($,$,#9032,#9136);
#102=ITEM_DEFINED_TRANSFORMATION($,$,#9032,#9137);
#103=ITEM_DEFINED_TRANSFORMATION($,$,#9032,#9138);
#104=ITEM_DEFINED_TRANSFORMATION($,$,#9032,#9139);
#105=ITEM_DEFINED_TRANSFORMATION($,$,#9032,#9140);
#106=ITEM_DEFINED_TRANSFORMATION($,$,#8980,#9141);
#107=ITEM_DEFINED_TRANSFORMATION($,$,#9032,#9142);
#108=ITEM_DEFINED_TRANSFORMATION($,$,#9032,#9143);
#109=ITEM_DEFINED_TRANSFORMATION($,$,#9032,#9144);
#110=ITEM_DEFINED_TRANSFORMATION($,$,#9032,#9145);
#111=ITEM_DEFINED_TRANSFORMATION($,$,#9032,#9146);
#112=ITEM_DEFINED_TRANSFORMATION($,$,#9032,#9147);
#113=ITEM_DEFINED_TRANSFORMATION($,$,#9032,#9148);
#114=ITEM_DEFINED_TRANSFORMATION($,$,#9032,#9149);
#115=ITEM_DEFINED_TRANSFORMATION($,$,#9056,#9150);
#116=ITEM_DEFINED_TRANSFORMATION($,$,#9056,#9151);
#117=ITEM_DEFINED_TRANSFORMATION($,$,#9056,#9152);
#118=ITEM_DEFINED_TRANSFORMATION($,$,#9056,#9153);
#119=ITEM_DEFINED_TRANSFORMATION($,$,#9155,#9361);
#120=ITEM_DEFINED_TRANSFORMATION($,$,#9176,#9362);
#121=ITEM_DEFINED_TRANSFORMATION($,$,#9180,#9363);
#122=ITEM_DEFINED_TRANSFORMATION($,$,#9190,#9364);
#123=ITEM_DEFINED_TRANSFORMATION($,$,#9216,#9365);
#124=ITEM_DEFINED_TRANSFORMATION($,$,#9243,#9366);
#125=ITEM_DEFINED_TRANSFORMATION($,$,#9260,#9367);
#126=ITEM_DEFINED_TRANSFORMATION($,$,#9275,#9368);
#127=ITEM_DEFINED_TRANSFORMATION($,$,#9275,#9369);
#128=ITEM_DEFINED_TRANSFORMATION($,$,#9275,#9370);
#129=ITEM_DEFINED_TRANSFORMATION($,$,#9284,#9371);
#130=ITEM_DEFINED_TRANSFORMATION($,$,#9295,#9372);
#131=ITEM_DEFINED_TRANSFORMATION($,$,#9305,#9373);
#132=ITEM_DEFINED_TRANSFORMATION($,$,#9315,#9374);
#133=ITEM_DEFINED_TRANSFORMATION($,$,#9336,#9375);
#134=ITEM_DEFINED_TRANSFORMATION($,$,#9345,#9376);
#135=ITEM_DEFINED_TRANSFORMATION($,$,#9336,#9377);
#136=ITEM_DEFINED_TRANSFORMATION($,$,#9345,#9378);
#137=ITEM_DEFINED_TRANSFORMATION($,$,#8385,#9379);
#138=ITEM_DEFINED_TRANSFORMATION($,$,#9154,#9380);
#139=(
REPRESENTATION_RELATIONSHIP($,$,#14597,#14596)
REPRESENTATION_RELATIONSHIP_WITH_TRANSFORMATION(#47)
SHAPE_REPRESENTATION_RELATIONSHIP()
);
#140=(
REPRESENTATION_RELATIONSHIP($,$,#14598,#14596)
REPRESENTATION_RELATIONSHIP_WITH_TRANSFORMATION(#48)
SHAPE_REPRESENTATION_RELATIONSHIP()
);
#141=(
REPRESENTATION_RELATIONSHIP($,$,#14611,#14610)
REPRESENTATION_RELATIONSHIP_WITH_TRANSFORMATION(#49)
SHAPE_REPRESENTATION_RELATIONSHIP()
);
#142=(
REPRESENTATION_RELATIONSHIP($,$,#14612,#14610)
REPRESENTATION_RELATIONSHIP_WITH_TRANSFORMATION(#50)
SHAPE_REPRESENTATION_RELATIONSHIP()
);
#143=(
REPRESENTATION_RELATIONSHIP($,$,#14585,#14584)
REPRESENTATION_RELATIONSHIP_WITH_TRANSFORMATION(#51)
SHAPE_REPRESENTATION_RELATIONSHIP()
);
#144=(
REPRESENTATION_RELATIONSHIP($,$,#14586,#14584)
REPRESENTATION_RELATIONSHIP_WITH_TRANSFORMATION(#52)
SHAPE_REPRESENTATION_RELATIONSHIP()
);
#145=(
REPRESENTATION_RELATIONSHIP($,$,#14587,#14584)
REPRESENTATION_RELATIONSHIP_WITH_TRANSFORMATION(#53)
SHAPE_REPRESENTATION_RELATIONSHIP()
);
#146=(
REPRESENTATION_RELATIONSHIP($,$,#14588,#14584)
REPRESENTATION_RELATIONSHIP_WITH_TRANSFORMATION(#54)
SHAPE_REPRESENTATION_RELATIONSHIP()
);
#147=(
REPRESENTATION_RELATIONSHIP($,$,#14589,#14584)
REPRESENTATION_RELATIONSHIP_WITH_TRANSFORMATION(#55)
SHAPE_REPRESENTATION_RELATIONSHIP()
);
#148=(
REPRESENTATION_RELATIONSHIP($,$,#14590,#14584)
REPRESENTATION_RELATIONSHIP_WITH_TRANSFORMATION(#56)
SHAPE_REPRESENTATION_RELATIONSHIP()
);
#149=(
REPRESENTATION_RELATIONSHIP($,$,#14591,#14584)
REPRESENTATION_RELATIONSHIP_WITH_TRANSFORMATION(#57)
SHAPE_REPRESENTATION_RELATIONSHIP()
);
#150=(
REPRESENTATION_RELATIONSHIP($,$,#14592,#14584)
REPRESENTATION_RELATIONSHIP_WITH_TRANSFORMATION(#58)
SHAPE_REPRESENTATION_RELATIONSHIP()
);
#151=(
REPRESENTATION_RELATIONSHIP($,$,#14593,#14584)
REPRESENTATION_RELATIONSHIP_WITH_TRANSFORMATION(#59)
SHAPE_REPRESENTATION_RELATIONSHIP()
);
#152=(
REPRESENTATION_RELATIONSHIP($,$,#14594,#14584)
REPRESENTATION_RELATIONSHIP_WITH_TRANSFORMATION(#60)
SHAPE_REPRESENTATION_RELATIONSHIP()
);
#153=(
REPRESENTATION_RELATIONSHIP($,$,#14595,#14584)
REPRESENTATION_RELATIONSHIP_WITH_TRANSFORMATION(#61)
SHAPE_REPRESENTATION_RELATIONSHIP()
);
#154=(
REPRESENTATION_RELATIONSHIP($,$,#14595,#14584)
REPRESENTATION_RELATIONSHIP_WITH_TRANSFORMATION(#62)
SHAPE_REPRESENTATION_RELATIONSHIP()
);
#155=(
REPRESENTATION_RELATIONSHIP($,$,#14596,#14584)
REPRESENTATION_RELATIONSHIP_WITH_TRANSFORMATION(#63)
SHAPE_REPRESENTATION_RELATIONSHIP()
);
#156=(
REPRESENTATION_RELATIONSHIP($,$,#14599,#14584)
REPRESENTATION_RELATIONSHIP_WITH_TRANSFORMATION(#64)
SHAPE_REPRESENTATION_RELATIONSHIP()
);
#157=(
REPRESENTATION_RELATIONSHIP($,$,#14594,#14584)
REPRESENTATION_RELATIONSHIP_WITH_TRANSFORMATION(#65)
SHAPE_REPRESENTATION_RELATIONSHIP()
);
#158=(
REPRESENTATION_RELATIONSHIP($,$,#14595,#14584)
REPRESENTATION_RELATIONSHIP_WITH_TRANSFORMATION(#66)
SHAPE_REPRESENTATION_RELATIONSHIP()
);
#159=(
REPRESENTATION_RELATIONSHIP($,$,#14595,#14584)
REPRESENTATION_RELATIONSHIP_WITH_TRANSFORMATION(#67)
SHAPE_REPRESENTATION_RELATIONSHIP()
);
#160=(
REPRESENTATION_RELATIONSHIP($,$,#14596,#14584)
REPRESENTATION_RELATIONSHIP_WITH_TRANSFORMATION(#68)
SHAPE_REPRESENTATION_RELATIONSHIP()
);
#161=(
REPRESENTATION_RELATIONSHIP($,$,#14599,#14584)
REPRESENTATION_RELATIONSHIP_WITH_TRANSFORMATION(#69)
SHAPE_REPRESENTATION_RELATIONSHIP()
);
#162=(
REPRESENTATION_RELATIONSHIP($,$,#14600,#14584)
REPRESENTATION_RELATIONSHIP_WITH_TRANSFORMATION(#70)
SHAPE_REPRESENTATION_RELATIONSHIP()
);
#163=(
REPRESENTATION_RELATIONSHIP($,$,#14601,#14584)
REPRESENTATION_RELATIONSHIP_WITH_TRANSFORMATION(#71)
SHAPE_REPRESENTATION_RELATIONSHIP()
);
#164=(
REPRESENTATION_RELATIONSHIP($,$,#14602,#14584)
REPRESENTATION_RELATIONSHIP_WITH_TRANSFORMATION(#72)
SHAPE_REPRESENTATION_RELATIONSHIP()
);
#165=(
REPRESENTATION_RELATIONSHIP($,$,#14603,#14584)
REPRESENTATION_RELATIONSHIP_WITH_TRANSFORMATION(#73)
SHAPE_REPRESENTATION_RELATIONSHIP()
);
#166=(
REPRESENTATION_RELATIONSHIP($,$,#14604,#14584)
REPRESENTATION_RELATIONSHIP_WITH_TRANSFORMATION(#74)
SHAPE_REPRESENTATION_RELATIONSHIP()
);
#167=(
REPRESENTATION_RELATIONSHIP($,$,#14603,#14584)
REPRESENTATION_RELATIONSHIP_WITH_TRANSFORMATION(#75)
SHAPE_REPRESENTATION_RELATIONSHIP()
);
#168=(
REPRESENTATION_RELATIONSHIP($,$,#14604,#14584)
REPRESENTATION_RELATIONSHIP_WITH_TRANSFORMATION(#76)
SHAPE_REPRESENTATION_RELATIONSHIP()
);
#169=(
REPRESENTATION_RELATIONSHIP($,$,#14602,#14584)
REPRESENTATION_RELATIONSHIP_WITH_TRANSFORMATION(#77)
SHAPE_REPRESENTATION_RELATIONSHIP()
);
#170=(
REPRESENTATION_RELATIONSHIP($,$,#14603,#14584)
REPRESENTATION_RELATIONSHIP_WITH_TRANSFORMATION(#78)
SHAPE_REPRESENTATION_RELATIONSHIP()
);
#171=(
REPRESENTATION_RELATIONSHIP($,$,#14604,#14584)
REPRESENTATION_RELATIONSHIP_WITH_TRANSFORMATION(#79)
SHAPE_REPRESENTATION_RELATIONSHIP()
);
#172=(
REPRESENTATION_RELATIONSHIP($,$,#14603,#14584)
REPRESENTATION_RELATIONSHIP_WITH_TRANSFORMATION(#80)
SHAPE_REPRESENTATION_RELATIONSHIP()
);
#173=(
REPRESENTATION_RELATIONSHIP($,$,#14604,#14584)
REPRESENTATION_RELATIONSHIP_WITH_TRANSFORMATION(#81)
SHAPE_REPRESENTATION_RELATIONSHIP()
);
#174=(
REPRESENTATION_RELATIONSHIP($,$,#14602,#14584)
REPRESENTATION_RELATIONSHIP_WITH_TRANSFORMATION(#82)
SHAPE_REPRESENTATION_RELATIONSHIP()
);
#175=(
REPRESENTATION_RELATIONSHIP($,$,#14603,#14584)
REPRESENTATION_RELATIONSHIP_WITH_TRANSFORMATION(#83)
SHAPE_REPRESENTATION_RELATIONSHIP()
);
#176=(
REPRESENTATION_RELATIONSHIP($,$,#14604,#14584)
REPRESENTATION_RELATIONSHIP_WITH_TRANSFORMATION(#84)
SHAPE_REPRESENTATION_RELATIONSHIP()
);
#177=(
REPRESENTATION_RELATIONSHIP($,$,#14603,#14584)
REPRESENTATION_RELATIONSHIP_WITH_TRANSFORMATION(#85)
SHAPE_REPRESENTATION_RELATIONSHIP()
);
#178=(
REPRESENTATION_RELATIONSHIP($,$,#14604,#14584)
REPRESENTATION_RELATIONSHIP_WITH_TRANSFORMATION(#86)
SHAPE_REPRESENTATION_RELATIONSHIP()
);
#179=(
REPRESENTATION_RELATIONSHIP($,$,#14602,#14584)
REPRESENTATION_RELATIONSHIP_WITH_TRANSFORMATION(#87)
SHAPE_REPRESENTATION_RELATIONSHIP()
);
#180=(
REPRESENTATION_RELATIONSHIP($,$,#14603,#14584)
REPRESENTATION_RELATIONSHIP_WITH_TRANSFORMATION(#88)
SHAPE_REPRESENTATION_RELATIONSHIP()
);
#181=(
REPRESENTATION_RELATIONSHIP($,$,#14604,#14584)
REPRESENTATION_RELATIONSHIP_WITH_TRANSFORMATION(#89)
SHAPE_REPRESENTATION_RELATIONSHIP()
);
#182=(
REPRESENTATION_RELATIONSHIP($,$,#14603,#14584)
REPRESENTATION_RELATIONSHIP_WITH_TRANSFORMATION(#90)
SHAPE_REPRESENTATION_RELATIONSHIP()
);
#183=(
REPRESENTATION_RELATIONSHIP($,$,#14604,#14584)
REPRESENTATION_RELATIONSHIP_WITH_TRANSFORMATION(#91)
SHAPE_REPRESENTATION_RELATIONSHIP()
);
#184=(
REPRESENTATION_RELATIONSHIP($,$,#14605,#14584)
REPRESENTATION_RELATIONSHIP_WITH_TRANSFORMATION(#92)
SHAPE_REPRESENTATION_RELATIONSHIP()
);
#185=(
REPRESENTATION_RELATIONSHIP($,$,#14606,#14584)
REPRESENTATION_RELATIONSHIP_WITH_TRANSFORMATION(#93)
SHAPE_REPRESENTATION_RELATIONSHIP()
);
#186=(
REPRESENTATION_RELATIONSHIP($,$,#14607,#14584)
REPRESENTATION_RELATIONSHIP_WITH_TRANSFORMATION(#94)
SHAPE_REPRESENTATION_RELATIONSHIP()
);
#187=(
REPRESENTATION_RELATIONSHIP($,$,#14608,#14584)
REPRESENTATION_RELATIONSHIP_WITH_TRANSFORMATION(#95)
SHAPE_REPRESENTATION_RELATIONSHIP()
);
#188=(
REPRESENTATION_RELATIONSHIP($,$,#14609,#14584)
REPRESENTATION_RELATIONSHIP_WITH_TRANSFORMATION(#96)
SHAPE_REPRESENTATION_RELATIONSHIP()
);
#189=(
REPRESENTATION_RELATIONSHIP($,$,#14610,#14584)
REPRESENTATION_RELATIONSHIP_WITH_TRANSFORMATION(#97)
SHAPE_REPRESENTATION_RELATIONSHIP()
);
#190=(
REPRESENTATION_RELATIONSHIP($,$,#14613,#14584)
REPRESENTATION_RELATIONSHIP_WITH_TRANSFORMATION(#98)
SHAPE_REPRESENTATION_RELATIONSHIP()
);
#191=(
REPRESENTATION_RELATIONSHIP($,$,#14613,#14584)
REPRESENTATION_RELATIONSHIP_WITH_TRANSFORMATION(#99)
SHAPE_REPRESENTATION_RELATIONSHIP()
);
#192=(
REPRESENTATION_RELATIONSHIP($,$,#14613,#14584)
REPRESENTATION_RELATIONSHIP_WITH_TRANSFORMATION(#100)
SHAPE_REPRESENTATION_RELATIONSHIP()
);
#193=(
REPRESENTATION_RELATIONSHIP($,$,#14613,#14584)
REPRESENTATION_RELATIONSHIP_WITH_TRANSFORMATION(#101)
SHAPE_REPRESENTATION_RELATIONSHIP()
);
#194=(
REPRESENTATION_RELATIONSHIP($,$,#14613,#14584)
REPRESENTATION_RELATIONSHIP_WITH_TRANSFORMATION(#102)
SHAPE_REPRESENTATION_RELATIONSHIP()
);
#195=(
REPRESENTATION_RELATIONSHIP($,$,#14613,#14584)
REPRESENTATION_RELATIONSHIP_WITH_TRANSFORMATION(#103)
SHAPE_REPRESENTATION_RELATIONSHIP()
);
#196=(
REPRESENTATION_RELATIONSHIP($,$,#14613,#14584)
REPRESENTATION_RELATIONSHIP_WITH_TRANSFORMATION(#104)
SHAPE_REPRESENTATION_RELATIONSHIP()
);
#197=(
REPRESENTATION_RELATIONSHIP($,$,#14613,#14584)
REPRESENTATION_RELATIONSHIP_WITH_TRANSFORMATION(#105)
SHAPE_REPRESENTATION_RELATIONSHIP()
);
#198=(
REPRESENTATION_RELATIONSHIP($,$,#14610,#14584)
REPRESENTATION_RELATIONSHIP_WITH_TRANSFORMATION(#106)
SHAPE_REPRESENTATION_RELATIONSHIP()
);
#199=(
REPRESENTATION_RELATIONSHIP($,$,#14613,#14584)
REPRESENTATION_RELATIONSHIP_WITH_TRANSFORMATION(#107)
SHAPE_REPRESENTATION_RELATIONSHIP()
);
#200=(
REPRESENTATION_RELATIONSHIP($,$,#14613,#14584)
REPRESENTATION_RELATIONSHIP_WITH_TRANSFORMATION(#108)
SHAPE_REPRESENTATION_RELATIONSHIP()
);
#201=(
REPRESENTATION_RELATIONSHIP($,$,#14613,#14584)
REPRESENTATION_RELATIONSHIP_WITH_TRANSFORMATION(#109)
SHAPE_REPRESENTATION_RELATIONSHIP()
);
#202=(
REPRESENTATION_RELATIONSHIP($,$,#14613,#14584)
REPRESENTATION_RELATIONSHIP_WITH_TRANSFORMATION(#110)
SHAPE_REPRESENTATION_RELATIONSHIP()
);
#203=(
REPRESENTATION_RELATIONSHIP($,$,#14613,#14584)
REPRESENTATION_RELATIONSHIP_WITH_TRANSFORMATION(#111)
SHAPE_REPRESENTATION_RELATIONSHIP()
);
#204=(
REPRESENTATION_RELATIONSHIP($,$,#14613,#14584)
REPRESENTATION_RELATIONSHIP_WITH_TRANSFORMATION(#112)
SHAPE_REPRESENTATION_RELATIONSHIP()
);
#205=(
REPRESENTATION_RELATIONSHIP($,$,#14613,#14584)
REPRESENTATION_RELATIONSHIP_WITH_TRANSFORMATION(#113)
SHAPE_REPRESENTATION_RELATIONSHIP()
);
#206=(
REPRESENTATION_RELATIONSHIP($,$,#14613,#14584)
REPRESENTATION_RELATIONSHIP_WITH_TRANSFORMATION(#114)
SHAPE_REPRESENTATION_RELATIONSHIP()
);
#207=(
REPRESENTATION_RELATIONSHIP($,$,#14614,#14584)
REPRESENTATION_RELATIONSHIP_WITH_TRANSFORMATION(#115)
SHAPE_REPRESENTATION_RELATIONSHIP()
);
#208=(
REPRESENTATION_RELATIONSHIP($,$,#14614,#14584)
REPRESENTATION_RELATIONSHIP_WITH_TRANSFORMATION(#116)
SHAPE_REPRESENTATION_RELATIONSHIP()
);
#209=(
REPRESENTATION_RELATIONSHIP($,$,#14614,#14584)
REPRESENTATION_RELATIONSHIP_WITH_TRANSFORMATION(#117)
SHAPE_REPRESENTATION_RELATIONSHIP()
);
#210=(
REPRESENTATION_RELATIONSHIP($,$,#14614,#14584)
REPRESENTATION_RELATIONSHIP_WITH_TRANSFORMATION(#118)
SHAPE_REPRESENTATION_RELATIONSHIP()
);
#211=(
REPRESENTATION_RELATIONSHIP($,$,#14616,#14615)
REPRESENTATION_RELATIONSHIP_WITH_TRANSFORMATION(#119)
SHAPE_REPRESENTATION_RELATIONSHIP()
);
#212=(
REPRESENTATION_RELATIONSHIP($,$,#14617,#14615)
REPRESENTATION_RELATIONSHIP_WITH_TRANSFORMATION(#120)
SHAPE_REPRESENTATION_RELATIONSHIP()
);
#213=(
REPRESENTATION_RELATIONSHIP($,$,#14618,#14615)
REPRESENTATION_RELATIONSHIP_WITH_TRANSFORMATION(#121)
SHAPE_REPRESENTATION_RELATIONSHIP()
);
#214=(
REPRESENTATION_RELATIONSHIP($,$,#14619,#14615)
REPRESENTATION_RELATIONSHIP_WITH_TRANSFORMATION(#122)
SHAPE_REPRESENTATION_RELATIONSHIP()
);
#215=(
REPRESENTATION_RELATIONSHIP($,$,#14620,#14615)
REPRESENTATION_RELATIONSHIP_WITH_TRANSFORMATION(#123)
SHAPE_REPRESENTATION_RELATIONSHIP()
);
#216=(
REPRESENTATION_RELATIONSHIP($,$,#14621,#14615)
REPRESENTATION_RELATIONSHIP_WITH_TRANSFORMATION(#124)
SHAPE_REPRESENTATION_RELATIONSHIP()
);
#217=(
REPRESENTATION_RELATIONSHIP($,$,#14622,#14615)
REPRESENTATION_RELATIONSHIP_WITH_TRANSFORMATION(#125)
SHAPE_REPRESENTATION_RELATIONSHIP()
);
#218=(
REPRESENTATION_RELATIONSHIP($,$,#14623,#14615)
REPRESENTATION_RELATIONSHIP_WITH_TRANSFORMATION(#126)
SHAPE_REPRESENTATION_RELATIONSHIP()
);
#219=(
REPRESENTATION_RELATIONSHIP($,$,#14623,#14615)
REPRESENTATION_RELATIONSHIP_WITH_TRANSFORMATION(#127)
SHAPE_REPRESENTATION_RELATIONSHIP()
);
#220=(
REPRESENTATION_RELATIONSHIP($,$,#14623,#14615)
REPRESENTATION_RELATIONSHIP_WITH_TRANSFORMATION(#128)
SHAPE_REPRESENTATION_RELATIONSHIP()
);
#221=(
REPRESENTATION_RELATIONSHIP($,$,#14624,#14615)
REPRESENTATION_RELATIONSHIP_WITH_TRANSFORMATION(#129)
SHAPE_REPRESENTATION_RELATIONSHIP()
);
#222=(
REPRESENTATION_RELATIONSHIP($,$,#14625,#14615)
REPRESENTATION_RELATIONSHIP_WITH_TRANSFORMATION(#130)
SHAPE_REPRESENTATION_RELATIONSHIP()
);
#223=(
REPRESENTATION_RELATIONSHIP($,$,#14626,#14615)
REPRESENTATION_RELATIONSHIP_WITH_TRANSFORMATION(#131)
SHAPE_REPRESENTATION_RELATIONSHIP()
);
#224=(
REPRESENTATION_RELATIONSHIP($,$,#14627,#14615)
REPRESENTATION_RELATIONSHIP_WITH_TRANSFORMATION(#132)
SHAPE_REPRESENTATION_RELATIONSHIP()
);
#225=(
REPRESENTATION_RELATIONSHIP($,$,#14628,#14615)
REPRESENTATION_RELATIONSHIP_WITH_TRANSFORMATION(#133)
SHAPE_REPRESENTATION_RELATIONSHIP()
);
#226=(
REPRESENTATION_RELATIONSHIP($,$,#14629,#14615)
REPRESENTATION_RELATIONSHIP_WITH_TRANSFORMATION(#134)
SHAPE_REPRESENTATION_RELATIONSHIP()
);
#227=(
REPRESENTATION_RELATIONSHIP($,$,#14628,#14615)
REPRESENTATION_RELATIONSHIP_WITH_TRANSFORMATION(#135)
SHAPE_REPRESENTATION_RELATIONSHIP()
);
#228=(
REPRESENTATION_RELATIONSHIP($,$,#14629,#14615)
REPRESENTATION_RELATIONSHIP_WITH_TRANSFORMATION(#136)
SHAPE_REPRESENTATION_RELATIONSHIP()
);
#229=(
REPRESENTATION_RELATIONSHIP($,$,#14584,#14583)
REPRESENTATION_RELATIONSHIP_WITH_TRANSFORMATION(#137)
SHAPE_REPRESENTATION_RELATIONSHIP()
);
#230=(
REPRESENTATION_RELATIONSHIP($,$,#14615,#14583)
REPRESENTATION_RELATIONSHIP_WITH_TRANSFORMATION(#138)
SHAPE_REPRESENTATION_RELATIONSHIP()
);
#231=CONTEXT_DEPENDENT_SHAPE_REPRESENTATION(#139,#14460);
#232=CONTEXT_DEPENDENT_SHAPE_REPRESENTATION(#140,#14461);
#233=CONTEXT_DEPENDENT_SHAPE_REPRESENTATION(#141,#14476);
#234=CONTEXT_DEPENDENT_SHAPE_REPRESENTATION(#142,#14477);
#235=CONTEXT_DEPENDENT_SHAPE_REPRESENTATION(#143,#14480);
#236=CONTEXT_DEPENDENT_SHAPE_REPRESENTATION(#144,#14481);
#237=CONTEXT_DEPENDENT_SHAPE_REPRESENTATION(#145,#14482);
#238=CONTEXT_DEPENDENT_SHAPE_REPRESENTATION(#146,#14483);
#239=CONTEXT_DEPENDENT_SHAPE_REPRESENTATION(#147,#14484);
#240=CONTEXT_DEPENDENT_SHAPE_REPRESENTATION(#148,#14485);
#241=CONTEXT_DEPENDENT_SHAPE_REPRESENTATION(#149,#14486);
#242=CONTEXT_DEPENDENT_SHAPE_REPRESENTATION(#150,#14487);
#243=CONTEXT_DEPENDENT_SHAPE_REPRESENTATION(#151,#14488);
#244=CONTEXT_DEPENDENT_SHAPE_REPRESENTATION(#152,#14489);
#245=CONTEXT_DEPENDENT_SHAPE_REPRESENTATION(#153,#14490);
#246=CONTEXT_DEPENDENT_SHAPE_REPRESENTATION(#154,#14491);
#247=CONTEXT_DEPENDENT_SHAPE_REPRESENTATION(#155,#14492);
#248=CONTEXT_DEPENDENT_SHAPE_REPRESENTATION(#156,#14493);
#249=CONTEXT_DEPENDENT_SHAPE_REPRESENTATION(#157,#14494);
#250=CONTEXT_DEPENDENT_SHAPE_REPRESENTATION(#158,#14495);
#251=CONTEXT_DEPENDENT_SHAPE_REPRESENTATION(#159,#14496);
#252=CONTEXT_DEPENDENT_SHAPE_REPRESENTATION(#160,#14497);
#253=CONTEXT_DEPENDENT_SHAPE_REPRESENTATION(#161,#14498);
#254=CONTEXT_DEPENDENT_SHAPE_REPRESENTATION(#162,#14499);
#255=CONTEXT_DEPENDENT_SHAPE_REPRESENTATION(#163,#14500);
#256=CONTEXT_DEPENDENT_SHAPE_REPRESENTATION(#164,#14501);
#257=CONTEXT_DEPENDENT_SHAPE_REPRESENTATION(#165,#14502);
#258=CONTEXT_DEPENDENT_SHAPE_REPRESENTATION(#166,#14503);
#259=CONTEXT_DEPENDENT_SHAPE_REPRESENTATION(#167,#14504);
#260=CONTEXT_DEPENDENT_SHAPE_REPRESENTATION(#168,#14505);
#261=CONTEXT_DEPENDENT_SHAPE_REPRESENTATION(#169,#14506);
#262=CONTEXT_DEPENDENT_SHAPE_REPRESENTATION(#170,#14507);
#263=CONTEXT_DEPENDENT_SHAPE_REPRESENTATION(#171,#14508);
#264=CONTEXT_DEPENDENT_SHAPE_REPRESENTATION(#172,#14509);
#265=CONTEXT_DEPENDENT_SHAPE_REPRESENTATION(#173,#14510);
#266=CONTEXT_DEPENDENT_SHAPE_REPRESENTATION(#174,#14511);
#267=CONTEXT_DEPENDENT_SHAPE_REPRESENTATION(#175,#14512);
#268=CONTEXT_DEPENDENT_SHAPE_REPRESENTATION(#176,#14513);
#269=CONTEXT_DEPENDENT_SHAPE_REPRESENTATION(#177,#14514);
#270=CONTEXT_DEPENDENT_SHAPE_REPRESENTATION(#178,#14515);
#271=CONTEXT_DEPENDENT_SHAPE_REPRESENTATION(#179,#14516);
#272=CONTEXT_DEPENDENT_SHAPE_REPRESENTATION(#180,#14517);
#273=CONTEXT_DEPENDENT_SHAPE_REPRESENTATION(#181,#14518);
#274=CONTEXT_DEPENDENT_SHAPE_REPRESENTATION(#182,#14519);
#275=CONTEXT_DEPENDENT_SHAPE_REPRESENTATION(#183,#14520);
#276=CONTEXT_DEPENDENT_SHAPE_REPRESENTATION(#184,#14521);
#277=CONTEXT_DEPENDENT_SHAPE_REPRESENTATION(#185,#14522);
#278=CONTEXT_DEPENDENT_SHAPE_REPRESENTATION(#186,#14523);
#279=CONTEXT_DEPENDENT_SHAPE_REPRESENTATION(#187,#14524);
#280=CONTEXT_DEPENDENT_SHAPE_REPRESENTATION(#188,#14525);
#281=CONTEXT_DEPENDENT_SHAPE_REPRESENTATION(#189,#14526);
#282=CONTEXT_DEPENDENT_SHAPE_REPRESENTATION(#190,#14527);
#283=CONTEXT_DEPENDENT_SHAPE_REPRESENTATION(#191,#14528);
#284=CONTEXT_DEPENDENT_SHAPE_REPRESENTATION(#192,#14529);
#285=CONTEXT_DEPENDENT_SHAPE_REPRESENTATION(#193,#14530);
#286=CONTEXT_DEPENDENT_SHAPE_REPRESENTATION(#194,#14531);
#287=CONTEXT_DEPENDENT_SHAPE_REPRESENTATION(#195,#14532);
#288=CONTEXT_DEPENDENT_SHAPE_REPRESENTATION(#196,#14533);
#289=CONTEXT_DEPENDENT_SHAPE_REPRESENTATION(#197,#14534);
#290=CONTEXT_DEPENDENT_SHAPE_REPRESENTATION(#198,#14535);
#291=CONTEXT_DEPENDENT_SHAPE_REPRESENTATION(#199,#14536);
#292=CONTEXT_DEPENDENT_SHAPE_REPRESENTATION(#200,#14537);
#293=CONTEXT_DEPENDENT_SHAPE_REPRESENTATION(#201,#14538);
#294=CONTEXT_DEPENDENT_SHAPE_REPRESENTATION(#202,#14539);
#295=CONTEXT_DEPENDENT_SHAPE_REPRESENTATION(#203,#14540);
#296=CONTEXT_DEPENDENT_SHAPE_REPRESENTATION(#204,#14541);
#297=CONTEXT_DEPENDENT_SHAPE_REPRESENTATION(#205,#14542);
#298=CONTEXT_DEPENDENT_SHAPE_REPRESENTATION(#206,#14543);
#299=CONTEXT_DEPENDENT_SHAPE_REPRESENTATION(#207,#14544);
#300=CONTEXT_DEPENDENT_SHAPE_REPRESENTATION(#208,#14545);
#301=CONTEXT_DEPENDENT_SHAPE_REPRESENTATION(#209,#14546);
#302=CONTEXT_DEPENDENT_SHAPE_REPRESENTATION(#210,#14547);
#303=CONTEXT_DEPENDENT_SHAPE_REPRESENTATION(#211,#14563);
#304=CONTEXT_DEPENDENT_SHAPE_REPRESENTATION(#212,#14564);
#305=CONTEXT_DEPENDENT_SHAPE_REPRESENTATION(#213,#14565);
#306=CONTEXT_DEPENDENT_SHAPE_REPRESENTATION(#214,#14566);
#307=CONTEXT_DEPENDENT_SHAPE_REPRESENTATION(#215,#14567);
#308=CONTEXT_DEPENDENT_SHAPE_REPRESENTATION(#216,#14568);
#309=CONTEXT_DEPENDENT_SHAPE_REPRESENTATION(#217,#14569);
#310=CONTEXT_DEPENDENT_SHAPE_REPRESENTATION(#218,#14570);
#311=CONTEXT_DEPENDENT_SHAPE_REPRESENTATION(#219,#14571);
#312=CONTEXT_DEPENDENT_SHAPE_REPRESENTATION(#220,#14572);
#313=CONTEXT_DEPENDENT_SHAPE_REPRESENTATION(#221,#14573);
#314=CONTEXT_DEPENDENT_SHAPE_REPRESENTATION(#222,#14574);
#315=CONTEXT_DEPENDENT_SHAPE_REPRESENTATION(#223,#14575);
#316=CONTEXT_DEPENDENT_SHAPE_REPRESENTATION(#224,#14576);
#317=CONTEXT_DEPENDENT_SHAPE_REPRESENTATION(#225,#14577);
#318=CONTEXT_DEPENDENT_SHAPE_REPRESENTATION(#226,#14578);
#319=CONTEXT_DEPENDENT_SHAPE_REPRESENTATION(#227,#14579);
#320=CONTEXT_DEPENDENT_SHAPE_REPRESENTATION(#228,#14580);
#321=CONTEXT_DEPENDENT_SHAPE_REPRESENTATION(#229,#14581);
#322=CONTEXT_DEPENDENT_SHAPE_REPRESENTATION(#230,#14582);
#323=NEXT_ASSEMBLY_USAGE_OCCURRENCE('Body:1','Body:1','Body:1',#14644,#14645,
'Body:1');
#324=NEXT_ASSEMBLY_USAGE_OCCURRENCE('Release collar:1',
'Release collar:1','Release collar:1',#14644,#14646,'Release collar:1');
#325=NEXT_ASSEMBLY_USAGE_OCCURRENCE('Steel sleeve:1','Steel sleeve:1',
'Steel sleeve:1',#14658,#14659,'Steel sleeve:1');
#326=NEXT_ASSEMBLY_USAGE_OCCURRENCE('Ball retainer (plastic):1',
'Ball retainer (plastic):1','Ball retainer (plastic):1',#14658,#14660,
'Ball retainer (plastic):1');
#327=NEXT_ASSEMBLY_USAGE_OCCURRENCE('Front cylinder cap:1',
'Front cylinder cap:1','Front cylinder cap:1',#14632,#14633,
'Front cylinder cap:1');
#328=NEXT_ASSEMBLY_USAGE_OCCURRENCE('Needle flow-control fitting:1',
'Needle flow-control fitting:1','Needle flow-control fitting:1',#14632,
#14634,'Needle flow-control fitting:1');
#329=NEXT_ASSEMBLY_USAGE_OCCURRENCE('Metering needle and grip:1',
'Metering needle and grip:1','Metering needle and grip:1',#14632,#14635,
'Metering needle and grip:1');
#330=NEXT_ASSEMBLY_USAGE_OCCURRENCE('Rear cylinder cap:1',
'Rear cylinder cap:1','Rear cylinder cap:1',#14632,#14636,
'Rear cylinder cap:1');
#331=NEXT_ASSEMBLY_USAGE_OCCURRENCE('Needle flow-control fitting (1):1',
'Needle flow-control fitting (1):1','Needle flow-control fitting (1):1',
#14632,#14637,'Needle flow-control fitting (1):1');
#332=NEXT_ASSEMBLY_USAGE_OCCURRENCE('Metering needle and grip (1):1',
'Metering needle and grip (1):1','Metering needle and grip (1):1',#14632,
#14638,'Metering needle and grip (1):1');
#333=NEXT_ASSEMBLY_USAGE_OCCURRENCE('Twenty millimetre bore barrel:1',
'Twenty millimetre bore barrel:1','Twenty millimetre bore barrel:1',#14632,
#14639,'Twenty millimetre bore barrel:1');
#334=NEXT_ASSEMBLY_USAGE_OCCURRENCE('Barrel end gasket:1',
'Barrel end gasket:1','Barrel end gasket:1',#14632,#14640,
'Barrel end gasket:1');
#335=NEXT_ASSEMBLY_USAGE_OCCURRENCE('Barrel end gasket (1):1',
'Barrel end gasket (1):1','Barrel end gasket (1):1',#14632,#14641,
'Barrel end gasket (1):1');
#336=NEXT_ASSEMBLY_USAGE_OCCURRENCE('Recessed cylinder mounting foot:2',
'Recessed cylinder mounting foot:2','Recessed cylinder mounting foot:2',
#14632,#14642,'Recessed cylinder mounting foot:2');
#337=NEXT_ASSEMBLY_USAGE_OCCURRENCE('Cap Screw - M5x20:2',
'Cap Screw - M5x20:2','Cap Screw - M5x20:2',#14632,#14643,
'Cap Screw - M5x20:2');
#338=NEXT_ASSEMBLY_USAGE_OCCURRENCE('Cap Screw - M5x20:3',
'Cap Screw - M5x20:3','Cap Screw - M5x20:3',#14632,#14643,
'Cap Screw - M5x20:3');
#339=NEXT_ASSEMBLY_USAGE_OCCURRENCE(
'Push-In Tube Fitting - 6 mm Tube, 1-8 Inch Tapered Pipe Thread:2',
'Push-In Tube Fitting - 6 mm Tube, 1-8 Inch Tapered Pipe Thread:2',
'Push-In Tube Fitting - 6 mm Tube, 1-8 Inch Tapered Pipe Thread:2',#14632,
#14644,
'Push-In Tube Fitting - 6 mm Tube, 1-8 Inch Tapered Pipe Thread:2');
#340=NEXT_ASSEMBLY_USAGE_OCCURRENCE('O-Ring:2','O-Ring:2','O-Ring:2',#14632,
#14647,'O-Ring:2');
#341=NEXT_ASSEMBLY_USAGE_OCCURRENCE('Recessed cylinder mounting foot:3',
'Recessed cylinder mounting foot:3','Recessed cylinder mounting foot:3',
#14632,#14642,'Recessed cylinder mounting foot:3');
#342=NEXT_ASSEMBLY_USAGE_OCCURRENCE('Cap Screw - M5x20:4',
'Cap Screw - M5x20:4','Cap Screw - M5x20:4',#14632,#14643,
'Cap Screw - M5x20:4');
#343=NEXT_ASSEMBLY_USAGE_OCCURRENCE('Cap Screw - M5x20:5',
'Cap Screw - M5x20:5','Cap Screw - M5x20:5',#14632,#14643,
'Cap Screw - M5x20:5');
#344=NEXT_ASSEMBLY_USAGE_OCCURRENCE(
'Push-In Tube Fitting - 6 mm Tube, 1-8 Inch Tapered Pipe Thread:3',
'Push-In Tube Fitting - 6 mm Tube, 1-8 Inch Tapered Pipe Thread:3',
'Push-In Tube Fitting - 6 mm Tube, 1-8 Inch Tapered Pipe Thread:3',#14632,
#14644,
'Push-In Tube Fitting - 6 mm Tube, 1-8 Inch Tapered Pipe Thread:3');
#345=NEXT_ASSEMBLY_USAGE_OCCURRENCE('O-Ring:3','O-Ring:3','O-Ring:3',#14632,
#14647,'O-Ring:3');
#346=NEXT_ASSEMBLY_USAGE_OCCURRENCE('Rod guide:2','Rod guide:2',
'Rod guide:2',#14632,#14648,'Rod guide:2');
#347=NEXT_ASSEMBLY_USAGE_OCCURRENCE('Rod seal:2','Rod seal:2',
'Rod seal:2',#14632,#14649,'Rod seal:2');
#348=NEXT_ASSEMBLY_USAGE_OCCURRENCE('M5 tie rod:2','M5 tie rod:2',
'M5 tie rod:2',#14632,#14650,'M5 tie rod:2');
#349=NEXT_ASSEMBLY_USAGE_OCCURRENCE('Flat Washer - M5:2',
'Flat Washer - M5:2','Flat Washer - M5:2',#14632,#14651,
'Flat Washer - M5:2');
#350=NEXT_ASSEMBLY_USAGE_OCCURRENCE('Hex Nut - M5:2','Hex Nut - M5:2',
'Hex Nut - M5:2',#14632,#14652,'Hex Nut - M5:2');
#351=NEXT_ASSEMBLY_USAGE_OCCURRENCE('Flat Washer - M5:3',
'Flat Washer - M5:3','Flat Washer - M5:3',#14632,#14651,
'Flat Washer - M5:3');
#352=NEXT_ASSEMBLY_USAGE_OCCURRENCE('Hex Nut - M5:3','Hex Nut - M5:3',
'Hex Nut - M5:3',#14632,#14652,'Hex Nut - M5:3');
#353=NEXT_ASSEMBLY_USAGE_OCCURRENCE('M5 tie rod:3','M5 tie rod:3',
'M5 tie rod:3',#14632,#14650,'M5 tie rod:3');
#354=NEXT_ASSEMBLY_USAGE_OCCURRENCE('Flat Washer - M5:4',
'Flat Washer - M5:4','Flat Washer - M5:4',#14632,#14651,
'Flat Washer - M5:4');
#355=NEXT_ASSEMBLY_USAGE_OCCURRENCE('Hex Nut - M5:4','Hex Nut - M5:4',
'Hex Nut - M5:4',#14632,#14652,'Hex Nut - M5:4');
#356=NEXT_ASSEMBLY_USAGE_OCCURRENCE('Flat Washer - M5:5',
'Flat Washer - M5:5','Flat Washer - M5:5',#14632,#14651,
'Flat Washer - M5:5');
#357=NEXT_ASSEMBLY_USAGE_OCCURRENCE('Hex Nut - M5:5','Hex Nut - M5:5',
'Hex Nut - M5:5',#14632,#14652,'Hex Nut - M5:5');
#358=NEXT_ASSEMBLY_USAGE_OCCURRENCE('M5 tie rod:4','M5 tie rod:4',
'M5 tie rod:4',#14632,#14650,'M5 tie rod:4');
#359=NEXT_ASSEMBLY_USAGE_OCCURRENCE('Flat Washer - M5:6',
'Flat Washer - M5:6','Flat Washer - M5:6',#14632,#14651,
'Flat Washer - M5:6');
#360=NEXT_ASSEMBLY_USAGE_OCCURRENCE('Hex Nut - M5:6','Hex Nut - M5:6',
'Hex Nut - M5:6',#14632,#14652,'Hex Nut - M5:6');
#361=NEXT_ASSEMBLY_USAGE_OCCURRENCE('Flat Washer - M5:7',
'Flat Washer - M5:7','Flat Washer - M5:7',#14632,#14651,
'Flat Washer - M5:7');
#362=NEXT_ASSEMBLY_USAGE_OCCURRENCE('Hex Nut - M5:7','Hex Nut - M5:7',
'Hex Nut - M5:7',#14632,#14652,'Hex Nut - M5:7');
#363=NEXT_ASSEMBLY_USAGE_OCCURRENCE('M5 tie rod:5','M5 tie rod:5',
'M5 tie rod:5',#14632,#14650,'M5 tie rod:5');
#364=NEXT_ASSEMBLY_USAGE_OCCURRENCE('Flat Washer - M5:8',
'Flat Washer - M5:8','Flat Washer - M5:8',#14632,#14651,
'Flat Washer - M5:8');
#365=NEXT_ASSEMBLY_USAGE_OCCURRENCE('Hex Nut - M5:8','Hex Nut - M5:8',
'Hex Nut - M5:8',#14632,#14652,'Hex Nut - M5:8');
#366=NEXT_ASSEMBLY_USAGE_OCCURRENCE('Flat Washer - M5:9',
'Flat Washer - M5:9','Flat Washer - M5:9',#14632,#14651,
'Flat Washer - M5:9');
#367=NEXT_ASSEMBLY_USAGE_OCCURRENCE('Hex Nut - M5:9','Hex Nut - M5:9',
'Hex Nut - M5:9',#14632,#14652,'Hex Nut - M5:9');
#368=NEXT_ASSEMBLY_USAGE_OCCURRENCE(
'Cylinder and guide mounting frame:1',
'Cylinder and guide mounting frame:1',
'Cylinder and guide mounting frame:1',#14632,#14653,
'Cylinder and guide mounting frame:1');
#369=NEXT_ASSEMBLY_USAGE_OCCURRENCE('Linear bearing retaining cap:1',
'Linear bearing retaining cap:1','Linear bearing retaining cap:1',#14632,
#14654,'Linear bearing retaining cap:1');
#370=NEXT_ASSEMBLY_USAGE_OCCURRENCE(
'Linear bearing retaining cap (1):1',
'Linear bearing retaining cap (1):1',
'Linear bearing retaining cap (1):1',#14632,#14655,
'Linear bearing retaining cap (1):1');
#371=NEXT_ASSEMBLY_USAGE_OCCURRENCE(
'Linear bearing retaining cap (2):1',
'Linear bearing retaining cap (2):1',
'Linear bearing retaining cap (2):1',#14632,#14656,
'Linear bearing retaining cap (2):1');
#372=NEXT_ASSEMBLY_USAGE_OCCURRENCE(
'Linear bearing retaining cap (3):1',
'Linear bearing retaining cap (3):1',
'Linear bearing retaining cap (3):1',#14632,#14657,
'Linear bearing retaining cap (3):1');
#373=NEXT_ASSEMBLY_USAGE_OCCURRENCE(
'Linear Ball Bushing - 12 x 21 x 30 mm:2',
'Linear Ball Bushing - 12 x 21 x 30 mm:2',
'Linear Ball Bushing - 12 x 21 x 30 mm:2',#14632,#14658,
'Linear Ball Bushing - 12 x 21 x 30 mm:2');
#374=NEXT_ASSEMBLY_USAGE_OCCURRENCE('M4x10 Cap Screw:2',
'M4x10 Cap Screw:2','M4x10 Cap Screw:2',#14632,#14661,
'M4x10 Cap Screw:2');
#375=NEXT_ASSEMBLY_USAGE_OCCURRENCE('M4x10 Cap Screw:3',
'M4x10 Cap Screw:3','M4x10 Cap Screw:3',#14632,#14661,
'M4x10 Cap Screw:3');
#376=NEXT_ASSEMBLY_USAGE_OCCURRENCE('M4x10 Cap Screw:4',
'M4x10 Cap Screw:4','M4x10 Cap Screw:4',#14632,#14661,
'M4x10 Cap Screw:4');
#377=NEXT_ASSEMBLY_USAGE_OCCURRENCE('M4x10 Cap Screw:5',
'M4x10 Cap Screw:5','M4x10 Cap Screw:5',#14632,#14661,
'M4x10 Cap Screw:5');
#378=NEXT_ASSEMBLY_USAGE_OCCURRENCE('M4x10 Cap Screw:6',
'M4x10 Cap Screw:6','M4x10 Cap Screw:6',#14632,#14661,
'M4x10 Cap Screw:6');
#379=NEXT_ASSEMBLY_USAGE_OCCURRENCE('M4x10 Cap Screw:7',
'M4x10 Cap Screw:7','M4x10 Cap Screw:7',#14632,#14661,
'M4x10 Cap Screw:7');
#380=NEXT_ASSEMBLY_USAGE_OCCURRENCE('M4x10 Cap Screw:8',
'M4x10 Cap Screw:8','M4x10 Cap Screw:8',#14632,#14661,
'M4x10 Cap Screw:8');
#381=NEXT_ASSEMBLY_USAGE_OCCURRENCE('M4x10 Cap Screw:9',
'M4x10 Cap Screw:9','M4x10 Cap Screw:9',#14632,#14661,
'M4x10 Cap Screw:9');
#382=NEXT_ASSEMBLY_USAGE_OCCURRENCE(
'Linear Ball Bushing - 12 x 21 x 30 mm:3',
'Linear Ball Bushing - 12 x 21 x 30 mm:3',
'Linear Ball Bushing - 12 x 21 x 30 mm:3',#14632,#14658,
'Linear Ball Bushing - 12 x 21 x 30 mm:3');
#383=NEXT_ASSEMBLY_USAGE_OCCURRENCE('M4x10 Cap Screw:10',
'M4x10 Cap Screw:10','M4x10 Cap Screw:10',#14632,#14661,
'M4x10 Cap Screw:10');
#384=NEXT_ASSEMBLY_USAGE_OCCURRENCE('M4x10 Cap Screw:11',
'M4x10 Cap Screw:11','M4x10 Cap Screw:11',#14632,#14661,
'M4x10 Cap Screw:11');
#385=NEXT_ASSEMBLY_USAGE_OCCURRENCE('M4x10 Cap Screw:12',
'M4x10 Cap Screw:12','M4x10 Cap Screw:12',#14632,#14661,
'M4x10 Cap Screw:12');
#386=NEXT_ASSEMBLY_USAGE_OCCURRENCE('M4x10 Cap Screw:13',
'M4x10 Cap Screw:13','M4x10 Cap Screw:13',#14632,#14661,
'M4x10 Cap Screw:13');
#387=NEXT_ASSEMBLY_USAGE_OCCURRENCE('M4x10 Cap Screw:14',
'M4x10 Cap Screw:14','M4x10 Cap Screw:14',#14632,#14661,
'M4x10 Cap Screw:14');
#388=NEXT_ASSEMBLY_USAGE_OCCURRENCE('M4x10 Cap Screw:15',
'M4x10 Cap Screw:15','M4x10 Cap Screw:15',#14632,#14661,
'M4x10 Cap Screw:15');
#389=NEXT_ASSEMBLY_USAGE_OCCURRENCE('M4x10 Cap Screw:16',
'M4x10 Cap Screw:16','M4x10 Cap Screw:16',#14632,#14661,
'M4x10 Cap Screw:16');
#390=NEXT_ASSEMBLY_USAGE_OCCURRENCE('M4x10 Cap Screw:17',
'M4x10 Cap Screw:17','M4x10 Cap Screw:17',#14632,#14661,
'M4x10 Cap Screw:17');
#391=NEXT_ASSEMBLY_USAGE_OCCURRENCE('Cylinder foot screw:2',
'Cylinder foot screw:2','Cylinder foot screw:2',#14632,#14662,
'Cylinder foot screw:2');
#392=NEXT_ASSEMBLY_USAGE_OCCURRENCE('Cylinder foot screw:3',
'Cylinder foot screw:3','Cylinder foot screw:3',#14632,#14662,
'Cylinder foot screw:3');
#393=NEXT_ASSEMBLY_USAGE_OCCURRENCE('Cylinder foot screw:4',
'Cylinder foot screw:4','Cylinder foot screw:4',#14632,#14662,
'Cylinder foot screw:4');
#394=NEXT_ASSEMBLY_USAGE_OCCURRENCE('Cylinder foot screw:5',
'Cylinder foot screw:5','Cylinder foot screw:5',#14632,#14662,
'Cylinder foot screw:5');
#395=NEXT_ASSEMBLY_USAGE_OCCURRENCE('Twenty millimetre piston:1',
'Twenty millimetre piston:1','Twenty millimetre piston:1',#14663,#14664,
'Twenty millimetre piston:1');
#396=NEXT_ASSEMBLY_USAGE_OCCURRENCE('Piston seal:1','Piston seal:1',
'Piston seal:1',#14663,#14665,'Piston seal:1');
#397=NEXT_ASSEMBLY_USAGE_OCCURRENCE('Piston rod:2','Piston rod:2',
'Piston rod:2',#14663,#14666,'Piston rod:2');
#398=NEXT_ASSEMBLY_USAGE_OCCURRENCE('Cap Screw - M4x16:2',
'Cap Screw - M4x16:2','Cap Screw - M4x16:2',#14663,#14667,
'Cap Screw - M4x16:2');
#399=NEXT_ASSEMBLY_USAGE_OCCURRENCE('Six-millimetre-pin rod clevis:2',
'Six-millimetre-pin rod clevis:2','Six-millimetre-pin rod clevis:2',#14663,
#14668,'Six-millimetre-pin rod clevis:2');
#400=NEXT_ASSEMBLY_USAGE_OCCURRENCE('Socket Set Screw - M4x6:2',
'Socket Set Screw - M4x6:2','Socket Set Screw - M4x6:2',#14663,#14669,
'Socket Set Screw - M4x6:2');
#401=NEXT_ASSEMBLY_USAGE_OCCURRENCE('Clevis Pin - 6x30:2',
'Clevis Pin - 6x30:2','Clevis Pin - 6x30:2',#14663,#14670,
'Clevis Pin - 6x30:2');
#402=NEXT_ASSEMBLY_USAGE_OCCURRENCE('Flat Washer - M6:2',
'Flat Washer - M6:2','Flat Washer - M6:2',#14663,#14671,
'Flat Washer - M6:2');
#403=NEXT_ASSEMBLY_USAGE_OCCURRENCE('Flat Washer - M6:3',
'Flat Washer - M6:3','Flat Washer - M6:3',#14663,#14671,
'Flat Washer - M6:3');
#404=NEXT_ASSEMBLY_USAGE_OCCURRENCE('Flat Washer - M6:4',
'Flat Washer - M6:4','Flat Washer - M6:4',#14663,#14671,
'Flat Washer - M6:4');
#405=NEXT_ASSEMBLY_USAGE_OCCURRENCE('Split Pin - 1.6x16:2',
'Split Pin - 1.6x16:2','Split Pin - 1.6x16:2',#14663,#14672,
'Split Pin - 1.6x16:2');
#406=NEXT_ASSEMBLY_USAGE_OCCURRENCE('Stepped guide rod:1',
'Stepped guide rod:1','Stepped guide rod:1',#14663,#14673,
'Stepped guide rod:1');
#407=NEXT_ASSEMBLY_USAGE_OCCURRENCE('Stepped guide rod (1):1',
'Stepped guide rod (1):1','Stepped guide rod (1):1',#14663,#14674,
'Stepped guide rod (1):1');
#408=NEXT_ASSEMBLY_USAGE_OCCURRENCE('Product stop crosshead:1',
'Product stop crosshead:1','Product stop crosshead:1',#14663,#14675,
'Product stop crosshead:1');
#409=NEXT_ASSEMBLY_USAGE_OCCURRENCE('Flat Washer - M6 (1):2',
'Flat Washer - M6 (1):2','Flat Washer - M6 (1):2',#14663,#14676,
'Flat Washer - M6 (1):2');
#410=NEXT_ASSEMBLY_USAGE_OCCURRENCE('Hex Nut - M6:2','Hex Nut - M6:2',
'Hex Nut - M6:2',#14663,#14677,'Hex Nut - M6:2');
#411=NEXT_ASSEMBLY_USAGE_OCCURRENCE('Flat Washer - M6 (1):3',
'Flat Washer - M6 (1):3','Flat Washer - M6 (1):3',#14663,#14676,
'Flat Washer - M6 (1):3');
#412=NEXT_ASSEMBLY_USAGE_OCCURRENCE('Hex Nut - M6:3','Hex Nut - M6:3',
'Hex Nut - M6:3',#14663,#14677,'Hex Nut - M6:3');
#413=NEXT_ASSEMBLY_USAGE_OCCURRENCE(
'Twenty millimetre bore cylinder and flow controls:1',
'Twenty millimetre bore cylinder and flow controls:1',
'Twenty millimetre bore cylinder and flow controls:1',#14631,#14632,
'Twenty millimetre bore cylinder and flow controls:1');
#414=NEXT_ASSEMBLY_USAGE_OCCURRENCE('Piston rod and clevis:1',
'Piston rod and clevis:1','Piston rod and clevis:1',#14631,#14663,
'Piston rod and clevis:1');
#415=ORIENTED_CLOSED_SHELL('',*,#7886,.F.);
#416=ORIENTED_CLOSED_SHELL('',*,#7902,.F.);
#417=ORIENTED_CLOSED_SHELL('',*,#7904,.F.);
#418=ORIENTED_CLOSED_SHELL('',*,#7910,.F.);
#419=BREP_WITH_VOIDS('Body1',#7885,(#415));
#420=BREP_WITH_VOIDS('Body1',#7903,(#416));
#421=BREP_WITH_VOIDS('Body1',#7905,(#417));
#422=BREP_WITH_VOIDS('Body1',#7909,(#418));
#423=CONICAL_SURFACE('',#8501,0.1,0.78539816339745);
#424=CONICAL_SURFACE('',#8503,0.25,0.321750554396641);
#425=CONICAL_SURFACE('',#8624,0.1,0.78539816339745);
#426=CONICAL_SURFACE('',#8626,0.25,0.321750554396641);
#427=CONICAL_SURFACE('',#8700,0.4,0.785398163397448);
#428=CONICAL_SURFACE('',#8704,0.41,0.785398163397448);
#429=CONICAL_SURFACE('',#8708,0.26,0.463647609000806);
#430=CONICAL_SURFACE('',#8712,0.225,0.785398163397448);
#431=CONICAL_SURFACE('',#8799,0.275,0.785398163397449);
#432=CONICAL_SURFACE('',#8810,0.47094010767585,1.0471975511966);
#433=CONICAL_SURFACE('',#8812,0.47094010767585,1.0471975511966);
#434=CONICAL_SURFACE('',#9045,0.325,0.785398163397448);
#435=CONICAL_SURFACE('',#9049,0.335,0.785398163397448);
#436=CONICAL_SURFACE('',#9053,0.21,0.463647609000806);
#437=CONICAL_SURFACE('',#9073,0.4,0.785398163397448);
#438=CONICAL_SURFACE('',#9077,0.41,0.785398163397448);
#439=CONICAL_SURFACE('',#9081,0.26,0.463647609000806);
#440=CONICAL_SURFACE('',#9085,0.225,0.785398163397448);
#441=CONICAL_SURFACE('',#9193,0.325,0.785398163397448);
#442=CONICAL_SURFACE('',#9197,0.335,0.785398163397448);
#443=CONICAL_SURFACE('',#9201,0.21,0.463647609000806);
#444=CONICAL_SURFACE('',#9205,0.18,0.785398163397448);
#445=CONICAL_SURFACE('',#9253,0.185,0.785398163397449);
#446=CONICAL_SURFACE('',#9257,0.1625,0.785398163397449);
#447=CONICAL_SURFACE('',#9264,0.475,0.785398163397448);
#448=CONICAL_SURFACE('',#9272,0.255,0.785398163397449);
#449=CONICAL_SURFACE('',#9346,0.576175134594813,1.0471975511966);
#450=CONICAL_SURFACE('',#9348,0.576175134594813,1.0471975511966);
#451=SHAPE_REPRESENTATION_RELATIONSHIP('SRR','None',#14585,#493);
#452=SHAPE_REPRESENTATION_RELATIONSHIP('SRR','None',#14586,#494);
#453=SHAPE_REPRESENTATION_RELATIONSHIP('SRR','None',#14587,#495);
#454=SHAPE_REPRESENTATION_RELATIONSHIP('SRR','None',#14588,#496);
#455=SHAPE_REPRESENTATION_RELATIONSHIP('SRR','None',#14589,#497);
#456=SHAPE_REPRESENTATION_RELATIONSHIP('SRR','None',#14590,#498);
#457=SHAPE_REPRESENTATION_RELATIONSHIP('SRR','None',#14591,#499);
#458=SHAPE_REPRESENTATION_RELATIONSHIP('SRR','None',#14592,#500);
#459=SHAPE_REPRESENTATION_RELATIONSHIP('SRR','None',#14593,#501);
#460=SHAPE_REPRESENTATION_RELATIONSHIP('SRR','None',#14594,#502);
#461=SHAPE_REPRESENTATION_RELATIONSHIP('SRR','None',#14595,#503);
#462=SHAPE_REPRESENTATION_RELATIONSHIP('SRR','None',#14597,#504);
#463=SHAPE_REPRESENTATION_RELATIONSHIP('SRR','None',#14598,#505);
#464=SHAPE_REPRESENTATION_RELATIONSHIP('SRR','None',#14599,#506);
#465=SHAPE_REPRESENTATION_RELATIONSHIP('SRR','None',#14600,#507);
#466=SHAPE_REPRESENTATION_RELATIONSHIP('SRR','None',#14601,#508);
#467=SHAPE_REPRESENTATION_RELATIONSHIP('SRR','None',#14602,#509);
#468=SHAPE_REPRESENTATION_RELATIONSHIP('SRR','None',#14603,#510);
#469=SHAPE_REPRESENTATION_RELATIONSHIP('SRR','None',#14604,#511);
#470=SHAPE_REPRESENTATION_RELATIONSHIP('SRR','None',#14605,#512);
#471=SHAPE_REPRESENTATION_RELATIONSHIP('SRR','None',#14606,#513);
#472=SHAPE_REPRESENTATION_RELATIONSHIP('SRR','None',#14607,#514);
#473=SHAPE_REPRESENTATION_RELATIONSHIP('SRR','None',#14608,#515);
#474=SHAPE_REPRESENTATION_RELATIONSHIP('SRR','None',#14609,#516);
#475=SHAPE_REPRESENTATION_RELATIONSHIP('SRR','None',#14611,#517);
#476=SHAPE_REPRESENTATION_RELATIONSHIP('SRR','None',#14612,#518);
#477=SHAPE_REPRESENTATION_RELATIONSHIP('SRR','None',#14613,#519);
#478=SHAPE_REPRESENTATION_RELATIONSHIP('SRR','None',#14614,#520);
#479=SHAPE_REPRESENTATION_RELATIONSHIP('SRR','None',#14616,#521);
#480=SHAPE_REPRESENTATION_RELATIONSHIP('SRR','None',#14617,#522);
#481=SHAPE_REPRESENTATION_RELATIONSHIP('SRR','None',#14618,#523);
#482=SHAPE_REPRESENTATION_RELATIONSHIP('SRR','None',#14619,#524);
#483=SHAPE_REPRESENTATION_RELATIONSHIP('SRR','None',#14620,#525);
#484=SHAPE_REPRESENTATION_RELATIONSHIP('SRR','None',#14621,#526);
#485=SHAPE_REPRESENTATION_RELATIONSHIP('SRR','None',#14622,#527);
#486=SHAPE_REPRESENTATION_RELATIONSHIP('SRR','None',#14623,#528);
#487=SHAPE_REPRESENTATION_RELATIONSHIP('SRR','None',#14624,#529);
#488=SHAPE_REPRESENTATION_RELATIONSHIP('SRR','None',#14625,#530);
#489=SHAPE_REPRESENTATION_RELATIONSHIP('SRR','None',#14626,#531);
#490=SHAPE_REPRESENTATION_RELATIONSHIP('SRR','None',#14627,#532);
#491=SHAPE_REPRESENTATION_RELATIONSHIP('SRR','None',#14628,#533);
#492=SHAPE_REPRESENTATION_RELATIONSHIP('SRR','None',#14629,#534);
#493=ADVANCED_BREP_SHAPE_REPRESENTATION('',(#577),#14347);
#494=ADVANCED_BREP_SHAPE_REPRESENTATION('',(#578),#14348);
#495=ADVANCED_BREP_SHAPE_REPRESENTATION('',(#579),#14349);
#496=ADVANCED_BREP_SHAPE_REPRESENTATION('',(#580),#14350);
#497=ADVANCED_BREP_SHAPE_REPRESENTATION('',(#581),#14351);
#498=ADVANCED_BREP_SHAPE_REPRESENTATION('',(#582),#14352);
#499=ADVANCED_BREP_SHAPE_REPRESENTATION('',(#583),#14353);
#500=ADVANCED_BREP_SHAPE_REPRESENTATION('',(#584),#14354);
#501=ADVANCED_BREP_SHAPE_REPRESENTATION('',(#585),#14355);
#502=ADVANCED_BREP_SHAPE_REPRESENTATION('',(#586),#14356);
#503=ADVANCED_BREP_SHAPE_REPRESENTATION('',(#419),#14357);
#504=ADVANCED_BREP_SHAPE_REPRESENTATION('',(#587),#14359);
#505=ADVANCED_BREP_SHAPE_REPRESENTATION('',(#588),#14360);
#506=ADVANCED_BREP_SHAPE_REPRESENTATION('',(#589),#14361);
#507=ADVANCED_BREP_SHAPE_REPRESENTATION('',(#590),#14362);
#508=ADVANCED_BREP_SHAPE_REPRESENTATION('',(#591),#14363);
#509=ADVANCED_BREP_SHAPE_REPRESENTATION('',(#592),#14364);
#510=ADVANCED_BREP_SHAPE_REPRESENTATION('',(#593),#14365);
#511=ADVANCED_BREP_SHAPE_REPRESENTATION('',(#594),#14366);
#512=ADVANCED_BREP_SHAPE_REPRESENTATION('',(#595),#14367);
#513=ADVANCED_BREP_SHAPE_REPRESENTATION('',(#596),#14368);
#514=ADVANCED_BREP_SHAPE_REPRESENTATION('',(#597),#14369);
#515=ADVANCED_BREP_SHAPE_REPRESENTATION('',(#598),#14370);
#516=ADVANCED_BREP_SHAPE_REPRESENTATION('',(#599),#14371);
#517=ADVANCED_BREP_SHAPE_REPRESENTATION('',(#600),#14373);
#518=ADVANCED_BREP_SHAPE_REPRESENTATION('',(#601),#14374);
#519=ADVANCED_BREP_SHAPE_REPRESENTATION('',(#420),#14375);
#520=ADVANCED_BREP_SHAPE_REPRESENTATION('',(#421),#14376);
#521=ADVANCED_BREP_SHAPE_REPRESENTATION('',(#602),#14378);
#522=ADVANCED_BREP_SHAPE_REPRESENTATION('',(#603),#14379);
#523=ADVANCED_BREP_SHAPE_REPRESENTATION('',(#604),#14380);
#524=ADVANCED_BREP_SHAPE_REPRESENTATION('',(#422),#14381);
#525=ADVANCED_BREP_SHAPE_REPRESENTATION('',(#605),#14382);
#526=ADVANCED_BREP_SHAPE_REPRESENTATION('',(#606),#14383);
#527=ADVANCED_BREP_SHAPE_REPRESENTATION('',(#607),#14384);
#528=ADVANCED_BREP_SHAPE_REPRESENTATION('',(#608),#14385);
#529=ADVANCED_BREP_SHAPE_REPRESENTATION('',(#609),#14386);
#530=ADVANCED_BREP_SHAPE_REPRESENTATION('',(#610),#14387);
#531=ADVANCED_BREP_SHAPE_REPRESENTATION('',(#611),#14388);
#532=ADVANCED_BREP_SHAPE_REPRESENTATION('',(#612),#14389);
#533=ADVANCED_BREP_SHAPE_REPRESENTATION('',(#613),#14390);
#534=ADVANCED_BREP_SHAPE_REPRESENTATION('',(#614),#14391);
#535=STYLED_ITEM('',(#14877),#577);
#536=STYLED_ITEM('',(#14884),#578);
#537=STYLED_ITEM('',(#14898),#579);
#538=STYLED_ITEM('',(#14877),#580);
#539=STYLED_ITEM('',(#14884),#581);
#540=STYLED_ITEM('',(#14898),#582);
#541=STYLED_ITEM('',(#14884),#583);
#542=STYLED_ITEM('',(#14884),#584);
#543=STYLED_ITEM('',(#14884),#585);
#544=STYLED_ITEM('',(#14877),#586);
#545=STYLED_ITEM('',(#14898),#419);
#546=STYLED_ITEM('',(#14870),#587);
#547=STYLED_ITEM('',(#14905),#588);
#548=STYLED_ITEM('',(#14898),#589);
#549=STYLED_ITEM('',(#14891),#590);
#550=STYLED_ITEM('',(#14898),#591);
#551=STYLED_ITEM('',(#14891),#592);
#552=STYLED_ITEM('',(#14898),#593);
#553=STYLED_ITEM('',(#14898),#594);
#554=STYLED_ITEM('',(#14870),#595);
#555=STYLED_ITEM('',(#14891),#596);
#556=STYLED_ITEM('',(#14891),#597);
#557=STYLED_ITEM('',(#14891),#598);
#558=STYLED_ITEM('',(#14891),#599);
#559=STYLED_ITEM('',(#14905),#600);
#560=STYLED_ITEM('',(#14884),#601);
#561=STYLED_ITEM('',(#14898),#420);
#562=STYLED_ITEM('',(#14898),#421);
#563=STYLED_ITEM('',(#14905),#602);
#564=STYLED_ITEM('',(#14898),#603);
#565=STYLED_ITEM('',(#14891),#604);
#566=STYLED_ITEM('',(#14898),#422);
#567=STYLED_ITEM('',(#14891),#605);
#568=STYLED_ITEM('',(#14898),#606);
#569=STYLED_ITEM('',(#14891),#607);
#570=STYLED_ITEM('',(#14898),#608);
#571=STYLED_ITEM('',(#14891),#609);
#572=STYLED_ITEM('',(#14891),#610);
#573=STYLED_ITEM('',(#14891),#611);
#574=STYLED_ITEM('',(#14891),#612);
#575=STYLED_ITEM('',(#14898),#613);
#576=STYLED_ITEM('',(#14898),#614);
#577=MANIFOLD_SOLID_BREP('Body1',#7875);
#578=MANIFOLD_SOLID_BREP('Body1',#7876);
#579=MANIFOLD_SOLID_BREP('Body1',#7877);
#580=MANIFOLD_SOLID_BREP('Body1',#7878);
#581=MANIFOLD_SOLID_BREP('Body1',#7879);
#582=MANIFOLD_SOLID_BREP('Body1',#7880);
#583=MANIFOLD_SOLID_BREP('Body1',#7881);
#584=MANIFOLD_SOLID_BREP('Body1',#7882);
#585=MANIFOLD_SOLID_BREP('Body1',#7883);
#586=MANIFOLD_SOLID_BREP('Body1',#7884);
#587=MANIFOLD_SOLID_BREP('Body1',#7887);
#588=MANIFOLD_SOLID_BREP('Body1',#7888);
#589=MANIFOLD_SOLID_BREP('Body1',#7889);
#590=MANIFOLD_SOLID_BREP('Body1',#7890);
#591=MANIFOLD_SOLID_BREP('Body1',#7891);
#592=MANIFOLD_SOLID_BREP('Body1',#7892);
#593=MANIFOLD_SOLID_BREP('Body1',#7893);
#594=MANIFOLD_SOLID_BREP('Body1',#7894);
#595=MANIFOLD_SOLID_BREP('Body1',#7895);
#596=MANIFOLD_SOLID_BREP('Body1',#7896);
#597=MANIFOLD_SOLID_BREP('Body1',#7897);
#598=MANIFOLD_SOLID_BREP('Body1',#7898);
#599=MANIFOLD_SOLID_BREP('Body1',#7899);
#600=MANIFOLD_SOLID_BREP('Body1',#7900);
#601=MANIFOLD_SOLID_BREP('Body1',#7901);
#602=MANIFOLD_SOLID_BREP('Body1',#7906);
#603=MANIFOLD_SOLID_BREP('Body1',#7907);
#604=MANIFOLD_SOLID_BREP('Body1',#7908);
#605=MANIFOLD_SOLID_BREP('Body1',#7911);
#606=MANIFOLD_SOLID_BREP('Body1',#7912);
#607=MANIFOLD_SOLID_BREP('Body1',#7913);
#608=MANIFOLD_SOLID_BREP('Body1',#7914);
#609=MANIFOLD_SOLID_BREP('Body1',#7915);
#610=MANIFOLD_SOLID_BREP('Body1',#7916);
#611=MANIFOLD_SOLID_BREP('Body1',#7917);
#612=MANIFOLD_SOLID_BREP('Body1',#7918);
#613=MANIFOLD_SOLID_BREP('Body1',#7919);
#614=MANIFOLD_SOLID_BREP('Body1',#7920);
#615=FACE_BOUND('',#1613,.T.);
#616=FACE_BOUND('',#1620,.T.);
#617=FACE_BOUND('',#1622,.T.);
#618=FACE_BOUND('',#1623,.T.);
#619=FACE_BOUND('',#1624,.T.);
#620=FACE_BOUND('',#1625,.T.);
#621=FACE_BOUND('',#1626,.T.);
#622=FACE_BOUND('',#1629,.T.);
#623=FACE_BOUND('',#1630,.T.);
#624=FACE_BOUND('',#1631,.T.);
#625=FACE_BOUND('',#1632,.T.);
#626=FACE_BOUND('',#1633,.T.);
#627=FACE_BOUND('',#1636,.T.);
#628=FACE_BOUND('',#1638,.T.);
#629=FACE_BOUND('',#1639,.T.);
#630=FACE_BOUND('',#1642,.T.);
#631=FACE_BOUND('',#1644,.T.);
#632=FACE_BOUND('',#1648,.T.);
#633=FACE_BOUND('',#1650,.T.);
#634=FACE_BOUND('',#1654,.T.);
#635=FACE_BOUND('',#1658,.T.);
#636=FACE_BOUND('',#1662,.T.);
#637=FACE_BOUND('',#1666,.T.);
#638=FACE_BOUND('',#1677,.T.);
#639=FACE_BOUND('',#1682,.T.);
#640=FACE_BOUND('',#1705,.T.);
#641=FACE_BOUND('',#1712,.T.);
#642=FACE_BOUND('',#1713,.T.);
#643=FACE_BOUND('',#1714,.T.);
#644=FACE_BOUND('',#1715,.T.);
#645=FACE_BOUND('',#1718,.T.);
#646=FACE_BOUND('',#1719,.T.);
#647=FACE_BOUND('',#1720,.T.);
#648=FACE_BOUND('',#1721,.T.);
#649=FACE_BOUND('',#1722,.T.);
#650=FACE_BOUND('',#1725,.T.);
#651=FACE_BOUND('',#1727,.T.);
#652=FACE_BOUND('',#1728,.T.);
#653=FACE_BOUND('',#1731,.T.);
#654=FACE_BOUND('',#1733,.T.);
#655=FACE_BOUND('',#1737,.T.);
#656=FACE_BOUND('',#1739,.T.);
#657=FACE_BOUND('',#1743,.T.);
#658=FACE_BOUND('',#1747,.T.);
#659=FACE_BOUND('',#1751,.T.);
#660=FACE_BOUND('',#1755,.T.);
#661=FACE_BOUND('',#1766,.T.);
#662=FACE_BOUND('',#1771,.T.);
#663=FACE_BOUND('',#1777,.T.);
#664=FACE_BOUND('',#1779,.T.);
#665=FACE_BOUND('',#1783,.T.);
#666=FACE_BOUND('',#1785,.T.);
#667=FACE_BOUND('',#1789,.T.);
#668=FACE_BOUND('',#1791,.T.);
#669=FACE_BOUND('',#1794,.T.);
#670=FACE_BOUND('',#1797,.T.);
#671=FACE_BOUND('',#1802,.T.);
#672=FACE_BOUND('',#1805,.T.);
#673=FACE_BOUND('',#1813,.T.);
#674=FACE_BOUND('',#1814,.T.);
#675=FACE_BOUND('',#1815,.T.);
#676=FACE_BOUND('',#1816,.T.);
#677=FACE_BOUND('',#1818,.T.);
#678=FACE_BOUND('',#1819,.T.);
#679=FACE_BOUND('',#1820,.T.);
#680=FACE_BOUND('',#1821,.T.);
#681=FACE_BOUND('',#1827,.T.);
#682=FACE_BOUND('',#1842,.T.);
#683=FACE_BOUND('',#1844,.T.);
#684=FACE_BOUND('',#1846,.T.);
#685=FACE_BOUND('',#1854,.T.);
#686=FACE_BOUND('',#1857,.T.);
#687=FACE_BOUND('',#1861,.T.);
#688=FACE_BOUND('',#1864,.T.);
#689=FACE_BOUND('',#1867,.T.);
#690=FACE_BOUND('',#1870,.T.);
#691=FACE_BOUND('',#1875,.T.);
#692=FACE_BOUND('',#1877,.T.);
#693=FACE_BOUND('',#1882,.T.);
#694=FACE_BOUND('',#1884,.T.);
#695=FACE_BOUND('',#1892,.T.);
#696=FACE_BOUND('',#1895,.T.);
#697=FACE_BOUND('',#1906,.T.);
#698=FACE_BOUND('',#1908,.T.);
#699=FACE_BOUND('',#1926,.T.);
#700=FACE_BOUND('',#1927,.T.);
#701=FACE_BOUND('',#1928,.T.);
#702=FACE_BOUND('',#1929,.T.);
#703=FACE_BOUND('',#1930,.T.);
#704=FACE_BOUND('',#1932,.T.);
#705=FACE_BOUND('',#1933,.T.);
#706=FACE_BOUND('',#1934,.T.);
#707=FACE_BOUND('',#1935,.T.);
#708=FACE_BOUND('',#1936,.T.);
#709=FACE_BOUND('',#1946,.T.);
#710=FACE_BOUND('',#1947,.T.);
#711=FACE_BOUND('',#1948,.T.);
#712=FACE_BOUND('',#1949,.T.);
#713=FACE_BOUND('',#1950,.T.);
#714=FACE_BOUND('',#1952,.T.);
#715=FACE_BOUND('',#1953,.T.);
#716=FACE_BOUND('',#1954,.T.);
#717=FACE_BOUND('',#1955,.T.);
#718=FACE_BOUND('',#1956,.T.);
#719=FACE_BOUND('',#1962,.T.);
#720=FACE_BOUND('',#1963,.T.);
#721=FACE_BOUND('',#1964,.T.);
#722=FACE_BOUND('',#1965,.T.);
#723=FACE_BOUND('',#1966,.T.);
#724=FACE_BOUND('',#1967,.T.);
#725=FACE_BOUND('',#1968,.T.);
#726=FACE_BOUND('',#1969,.T.);
#727=FACE_BOUND('',#1970,.T.);
#728=FACE_BOUND('',#1971,.T.);
#729=FACE_BOUND('',#1973,.T.);
#730=FACE_BOUND('',#1974,.T.);
#731=FACE_BOUND('',#1975,.T.);
#732=FACE_BOUND('',#1976,.T.);
#733=FACE_BOUND('',#1977,.T.);
#734=FACE_BOUND('',#1978,.T.);
#735=FACE_BOUND('',#1979,.T.);
#736=FACE_BOUND('',#1980,.T.);
#737=FACE_BOUND('',#1988,.T.);
#738=FACE_BOUND('',#1989,.T.);
#739=FACE_BOUND('',#1990,.T.);
#740=FACE_BOUND('',#1991,.T.);
#741=FACE_BOUND('',#1992,.T.);
#742=FACE_BOUND('',#1994,.T.);
#743=FACE_BOUND('',#1995,.T.);
#744=FACE_BOUND('',#1996,.T.);
#745=FACE_BOUND('',#1997,.T.);
#746=FACE_BOUND('',#1998,.T.);
#747=FACE_BOUND('',#2006,.T.);
#748=FACE_BOUND('',#2007,.T.);
#749=FACE_BOUND('',#2008,.T.);
#750=FACE_BOUND('',#2009,.T.);
#751=FACE_BOUND('',#2010,.T.);
#752=FACE_BOUND('',#2012,.T.);
#753=FACE_BOUND('',#2013,.T.);
#754=FACE_BOUND('',#2014,.T.);
#755=FACE_BOUND('',#2015,.T.);
#756=FACE_BOUND('',#2016,.T.);
#757=FACE_BOUND('',#2024,.T.);
#758=FACE_BOUND('',#2025,.T.);
#759=FACE_BOUND('',#2026,.T.);
#760=FACE_BOUND('',#2027,.T.);
#761=FACE_BOUND('',#2028,.T.);
#762=FACE_BOUND('',#2030,.T.);
#763=FACE_BOUND('',#2031,.T.);
#764=FACE_BOUND('',#2032,.T.);
#765=FACE_BOUND('',#2033,.T.);
#766=FACE_BOUND('',#2034,.T.);
#767=FACE_BOUND('',#2042,.T.);
#768=FACE_BOUND('',#2043,.T.);
#769=FACE_BOUND('',#2044,.T.);
#770=FACE_BOUND('',#2045,.T.);
#771=FACE_BOUND('',#2046,.T.);
#772=FACE_BOUND('',#2048,.T.);
#773=FACE_BOUND('',#2049,.T.);
#774=FACE_BOUND('',#2050,.T.);
#775=FACE_BOUND('',#2051,.T.);
#776=FACE_BOUND('',#2052,.T.);
#777=FACE_BOUND('',#2059,.T.);
#778=FACE_BOUND('',#2062,.T.);
#779=FACE_BOUND('',#2065,.T.);
#780=FACE_BOUND('',#2068,.T.);
#781=FACE_BOUND('',#2071,.T.);
#782=FACE_BOUND('',#2074,.T.);
#783=FACE_BOUND('',#2076,.T.);
#784=FACE_BOUND('',#2082,.T.);
#785=FACE_BOUND('',#2084,.T.);
#786=FACE_BOUND('',#2086,.T.);
#787=FACE_BOUND('',#2088,.T.);
#788=FACE_BOUND('',#2103,.T.);
#789=FACE_BOUND('',#2115,.T.);
#790=FACE_BOUND('',#2123,.T.);
#791=FACE_BOUND('',#2129,.T.);
#792=FACE_BOUND('',#2132,.T.);
#793=FACE_BOUND('',#2134,.T.);
#794=FACE_BOUND('',#2139,.T.);
#795=FACE_BOUND('',#2141,.T.);
#796=FACE_BOUND('',#2147,.T.);
#797=FACE_BOUND('',#2154,.T.);
#798=FACE_BOUND('',#2173,.T.);
#799=FACE_BOUND('',#2175,.T.);
#800=FACE_BOUND('',#2177,.T.);
#801=FACE_BOUND('',#2179,.T.);
#802=FACE_BOUND('',#2184,.T.);
#803=FACE_BOUND('',#2186,.T.);
#804=FACE_BOUND('',#2188,.T.);
#805=FACE_BOUND('',#2190,.T.);
#806=FACE_BOUND('',#2199,.T.);
#807=FACE_BOUND('',#2209,.T.);
#808=FACE_BOUND('',#2211,.T.);
#809=FACE_BOUND('',#2217,.T.);
#810=FACE_BOUND('',#2219,.T.);
#811=FACE_BOUND('',#2221,.T.);
#812=FACE_BOUND('',#2231,.T.);
#813=FACE_BOUND('',#2237,.T.);
#814=FACE_BOUND('',#2243,.T.);
#815=FACE_BOUND('',#2246,.T.);
#816=FACE_BOUND('',#2249,.T.);
#817=FACE_BOUND('',#2250,.T.);
#818=FACE_BOUND('',#2251,.T.);
#819=FACE_BOUND('',#2254,.T.);
#820=FACE_BOUND('',#2255,.T.);
#821=FACE_BOUND('',#2262,.T.);
#822=FACE_BOUND('',#2264,.T.);
#823=FACE_BOUND('',#2275,.T.);
#824=FACE_BOUND('',#2277,.T.);
#825=ELLIPSE('',#8400,0.282842712474619,0.2);
#826=ELLIPSE('',#8401,0.282842712474619,0.2);
#827=ELLIPSE('',#8403,0.282842712474619,0.2);
#828=ELLIPSE('',#8404,0.282842712474619,0.2);
#829=ELLIPSE('',#8408,0.282842712474619,0.2);
#830=ELLIPSE('',#8410,0.282842712474619,0.2);
#831=ELLIPSE('',#8412,0.282842712474619,0.2);
#832=ELLIPSE('',#8530,0.282842712474618,0.2);
#833=ELLIPSE('',#8531,0.282842712474618,0.2);
#834=ELLIPSE('',#8532,0.282842712474618,0.2);
#835=ELLIPSE('',#8535,0.282842712474618,0.2);
#836=ELLIPSE('',#8536,0.282842712474618,0.2);
#837=ELLIPSE('',#8538,0.282842712474618,0.2);
#838=ELLIPSE('',#8539,0.282842712474618,0.2);
#839=PLANE('',#8390);
#840=PLANE('',#8394);
#841=PLANE('',#8395);
#842=PLANE('',#8397);
#843=PLANE('',#8413);
#844=PLANE('',#8415);
#845=PLANE('',#8416);
#846=PLANE('',#8418);
#847=PLANE('',#8429);
#848=PLANE('',#8433);
#849=PLANE('',#8449);
#850=PLANE('',#8450);
#851=PLANE('',#8451);
#852=PLANE('',#8452);
#853=PLANE('',#8453);
#854=PLANE('',#8454);
#855=PLANE('',#8455);
#856=PLANE('',#8460);
#857=PLANE('',#8461);
#858=PLANE('',#8469);
#859=PLANE('',#8471);
#860=PLANE('',#8476);
#861=PLANE('',#8478);
#862=PLANE('',#8479);
#863=PLANE('',#8480);
#864=PLANE('',#8481);
#865=PLANE('',#8482);
#866=PLANE('',#8483);
#867=PLANE('',#8484);
#868=PLANE('',#8485);
#869=PLANE('',#8486);
#870=PLANE('',#8488);
#871=PLANE('',#8489);
#872=PLANE('',#8490);
#873=PLANE('',#8491);
#874=PLANE('',#8492);
#875=PLANE('',#8493);
#876=PLANE('',#8494);
#877=PLANE('',#8499);
#878=PLANE('',#8507);
#879=PLANE('',#8511);
#880=PLANE('',#8516);
#881=PLANE('',#8520);
#882=PLANE('',#8521);
#883=PLANE('',#8523);
#884=PLANE('',#8525);
#885=PLANE('',#8540);
#886=PLANE('',#8542);
#887=PLANE('',#8544);
#888=PLANE('',#8546);
#889=PLANE('',#8552);
#890=PLANE('',#8558);
#891=PLANE('',#8573);
#892=PLANE('',#8574);
#893=PLANE('',#8575);
#894=PLANE('',#8576);
#895=PLANE('',#8577);
#896=PLANE('',#8578);
#897=PLANE('',#8583);
#898=PLANE('',#8584);
#899=PLANE('',#8592);
#900=PLANE('',#8594);
#901=PLANE('',#8599);
#902=PLANE('',#8601);
#903=PLANE('',#8602);
#904=PLANE('',#8603);
#905=PLANE('',#8604);
#906=PLANE('',#8605);
#907=PLANE('',#8606);
#908=PLANE('',#8607);
#909=PLANE('',#8608);
#910=PLANE('',#8609);
#911=PLANE('',#8611);
#912=PLANE('',#8612);
#913=PLANE('',#8613);
#914=PLANE('',#8614);
#915=PLANE('',#8615);
#916=PLANE('',#8616);
#917=PLANE('',#8617);
#918=PLANE('',#8622);
#919=PLANE('',#8630);
#920=PLANE('',#8634);
#921=PLANE('',#8642);
#922=PLANE('',#8643);
#923=PLANE('',#8651);
#924=PLANE('',#8652);
#925=PLANE('',#8660);
#926=PLANE('',#8661);
#927=PLANE('',#8666);
#928=PLANE('',#8671);
#929=PLANE('',#8680);
#930=PLANE('',#8685);
#931=PLANE('',#8691);
#932=PLANE('',#8692);
#933=PLANE('',#8693);
#934=PLANE('',#8694);
#935=PLANE('',#8695);
#936=PLANE('',#8696);
#937=PLANE('',#8698);
#938=PLANE('',#8706);
#939=PLANE('',#8714);
#940=PLANE('',#8715);
#941=PLANE('',#8716);
#942=PLANE('',#8717);
#943=PLANE('',#8718);
#944=PLANE('',#8719);
#945=PLANE('',#8720);
#946=PLANE('',#8721);
#947=PLANE('',#8722);
#948=PLANE('',#8728);
#949=PLANE('',#8730);
#950=PLANE('',#8732);
#951=PLANE('',#8734);
#952=PLANE('',#8735);
#953=PLANE('',#8736);
#954=PLANE('',#8737);
#955=PLANE('',#8738);
#956=PLANE('',#8739);
#957=PLANE('',#8740);
#958=PLANE('',#8744);
#959=PLANE('',#8749);
#960=PLANE('',#8753);
#961=PLANE('',#8758);
#962=PLANE('',#8762);
#963=PLANE('',#8775);
#964=PLANE('',#8777);
#965=PLANE('',#8786);
#966=PLANE('',#8787);
#967=PLANE('',#8796);
#968=PLANE('',#8797);
#969=PLANE('',#8804);
#970=PLANE('',#8808);
#971=PLANE('',#8814);
#972=PLANE('',#8815);
#973=PLANE('',#8816);
#974=PLANE('',#8820);
#975=PLANE('',#8821);
#976=PLANE('',#8822);
#977=PLANE('',#8823);
#978=PLANE('',#8824);
#979=PLANE('',#8865);
#980=PLANE('',#8866);
#981=PLANE('',#8867);
#982=PLANE('',#8868);
#983=PLANE('',#8869);
#984=PLANE('',#8885);
#985=PLANE('',#8886);
#986=PLANE('',#8887);
#987=PLANE('',#8888);
#988=PLANE('',#8889);
#989=PLANE('',#8890);
#990=PLANE('',#8891);
#991=PLANE('',#8892);
#992=PLANE('',#8893);
#993=PLANE('',#8894);
#994=PLANE('',#8895);
#995=PLANE('',#8915);
#996=PLANE('',#8916);
#997=PLANE('',#8936);
#998=PLANE('',#8937);
#999=PLANE('',#8957);
#1000=PLANE('',#8958);
#1001=PLANE('',#8978);
#1002=PLANE('',#8979);
#1003=PLANE('',#8982);
#1004=PLANE('',#8984);
#1005=PLANE('',#8985);
#1006=PLANE('',#8987);
#1007=PLANE('',#8988);
#1008=PLANE('',#8989);
#1009=PLANE('',#8994);
#1010=PLANE('',#8998);
#1011=PLANE('',#9002);
#1012=PLANE('',#9006);
#1013=PLANE('',#9010);
#1014=PLANE('',#9014);
#1015=PLANE('',#9017);
#1016=PLANE('',#9018);
#1017=PLANE('',#9021);
#1018=PLANE('',#9022);
#1019=PLANE('',#9027);
#1020=PLANE('',#9033);
#1021=PLANE('',#9034);
#1022=PLANE('',#9035);
#1023=PLANE('',#9036);
#1024=PLANE('',#9037);
#1025=PLANE('',#9038);
#1026=PLANE('',#9039);
#1027=PLANE('',#9040);
#1028=PLANE('',#9041);
#1029=PLANE('',#9043);
#1030=PLANE('',#9051);
#1031=PLANE('',#9057);
#1032=PLANE('',#9058);
#1033=PLANE('',#9059);
#1034=PLANE('',#9060);
#1035=PLANE('',#9061);
#1036=PLANE('',#9062);
#1037=PLANE('',#9063);
#1038=PLANE('',#9064);
#1039=PLANE('',#9065);
#1040=PLANE('',#9070);
#1041=PLANE('',#9071);
#1042=PLANE('',#9079);
#1043=PLANE('',#9159);
#1044=PLANE('',#9164);
#1045=PLANE('',#9166);
#1046=PLANE('',#9174);
#1047=PLANE('',#9175);
#1048=PLANE('',#9184);
#1049=PLANE('',#9188);
#1050=PLANE('',#9189);
#1051=PLANE('',#9191);
#1052=PLANE('',#9199);
#1053=PLANE('',#9207);
#1054=PLANE('',#9208);
#1055=PLANE('',#9209);
#1056=PLANE('',#9210);
#1057=PLANE('',#9211);
#1058=PLANE('',#9212);
#1059=PLANE('',#9213);
#1060=PLANE('',#9214);
#1061=PLANE('',#9215);
#1062=PLANE('',#9223);
#1063=PLANE('',#9229);
#1064=PLANE('',#9233);
#1065=PLANE('',#9234);
#1066=PLANE('',#9235);
#1067=PLANE('',#9236);
#1068=PLANE('',#9237);
#1069=PLANE('',#9238);
#1070=PLANE('',#9239);
#1071=PLANE('',#9240);
#1072=PLANE('',#9241);
#1073=PLANE('',#9242);
#1074=PLANE('',#9244);
#1075=PLANE('',#9245);
#1076=PLANE('',#9246);
#1077=PLANE('',#9247);
#1078=PLANE('',#9248);
#1079=PLANE('',#9249);
#1080=PLANE('',#9250);
#1081=PLANE('',#9251);
#1082=PLANE('',#9259);
#1083=PLANE('',#9262);
#1084=PLANE('',#9268);
#1085=PLANE('',#9274);
#1086=PLANE('',#9282);
#1087=PLANE('',#9283);
#1088=PLANE('',#9288);
#1089=PLANE('',#9290);
#1090=PLANE('',#9294);
#1091=PLANE('',#9299);
#1092=PLANE('',#9303);
#1093=PLANE('',#9304);
#1094=PLANE('',#9309);
#1095=PLANE('',#9313);
#1096=PLANE('',#9314);
#1097=PLANE('',#9325);
#1098=PLANE('',#9326);
#1099=PLANE('',#9327);
#1100=PLANE('',#9328);
#1101=PLANE('',#9329);
#1102=PLANE('',#9330);
#1103=PLANE('',#9331);
#1104=PLANE('',#9332);
#1105=PLANE('',#9333);
#1106=PLANE('',#9334);
#1107=PLANE('',#9335);
#1108=PLANE('',#9343);
#1109=PLANE('',#9344);
#1110=PLANE('',#9350);
#1111=PLANE('',#9351);
#1112=PLANE('',#9352);
#1113=PLANE('',#9356);
#1114=PLANE('',#9357);
#1115=PLANE('',#9358);
#1116=PLANE('',#9359);
#1117=PLANE('',#9360);
#1118=FACE_OUTER_BOUND('',#1593,.T.);
#1119=FACE_OUTER_BOUND('',#1594,.T.);
#1120=FACE_OUTER_BOUND('',#1595,.T.);
#1121=FACE_OUTER_BOUND('',#1596,.T.);
#1122=FACE_OUTER_BOUND('',#1597,.T.);
#1123=FACE_OUTER_BOUND('',#1598,.T.);
#1124=FACE_OUTER_BOUND('',#1599,.T.);
#1125=FACE_OUTER_BOUND('',#1600,.T.);
#1126=FACE_OUTER_BOUND('',#1601,.T.);
#1127=FACE_OUTER_BOUND('',#1602,.T.);
#1128=FACE_OUTER_BOUND('',#1603,.T.);
#1129=FACE_OUTER_BOUND('',#1604,.T.);
#1130=FACE_OUTER_BOUND('',#1605,.T.);
#1131=FACE_OUTER_BOUND('',#1606,.T.);
#1132=FACE_OUTER_BOUND('',#1607,.T.);
#1133=FACE_OUTER_BOUND('',#1608,.T.);
#1134=FACE_OUTER_BOUND('',#1609,.T.);
#1135=FACE_OUTER_BOUND('',#1610,.T.);
#1136=FACE_OUTER_BOUND('',#1611,.T.);
#1137=FACE_OUTER_BOUND('',#1612,.T.);
#1138=FACE_OUTER_BOUND('',#1614,.T.);
#1139=FACE_OUTER_BOUND('',#1615,.T.);
#1140=FACE_OUTER_BOUND('',#1616,.T.);
#1141=FACE_OUTER_BOUND('',#1617,.T.);
#1142=FACE_OUTER_BOUND('',#1618,.T.);
#1143=FACE_OUTER_BOUND('',#1619,.T.);
#1144=FACE_OUTER_BOUND('',#1621,.T.);
#1145=FACE_OUTER_BOUND('',#1627,.T.);
#1146=FACE_OUTER_BOUND('',#1628,.T.);
#1147=FACE_OUTER_BOUND('',#1634,.T.);
#1148=FACE_OUTER_BOUND('',#1635,.T.);
#1149=FACE_OUTER_BOUND('',#1637,.T.);
#1150=FACE_OUTER_BOUND('',#1640,.T.);
#1151=FACE_OUTER_BOUND('',#1641,.T.);
#1152=FACE_OUTER_BOUND('',#1643,.T.);
#1153=FACE_OUTER_BOUND('',#1645,.T.);
#1154=FACE_OUTER_BOUND('',#1646,.T.);
#1155=FACE_OUTER_BOUND('',#1647,.T.);
#1156=FACE_OUTER_BOUND('',#1649,.T.);
#1157=FACE_OUTER_BOUND('',#1651,.T.);
#1158=FACE_OUTER_BOUND('',#1652,.T.);
#1159=FACE_OUTER_BOUND('',#1653,.T.);
#1160=FACE_OUTER_BOUND('',#1655,.T.);
#1161=FACE_OUTER_BOUND('',#1656,.T.);
#1162=FACE_OUTER_BOUND('',#1657,.T.);
#1163=FACE_OUTER_BOUND('',#1659,.T.);
#1164=FACE_OUTER_BOUND('',#1660,.T.);
#1165=FACE_OUTER_BOUND('',#1661,.T.);
#1166=FACE_OUTER_BOUND('',#1663,.T.);
#1167=FACE_OUTER_BOUND('',#1664,.T.);
#1168=FACE_OUTER_BOUND('',#1665,.T.);
#1169=FACE_OUTER_BOUND('',#1667,.T.);
#1170=FACE_OUTER_BOUND('',#1668,.T.);
#1171=FACE_OUTER_BOUND('',#1669,.T.);
#1172=FACE_OUTER_BOUND('',#1670,.T.);
#1173=FACE_OUTER_BOUND('',#1671,.T.);
#1174=FACE_OUTER_BOUND('',#1672,.T.);
#1175=FACE_OUTER_BOUND('',#1673,.T.);
#1176=FACE_OUTER_BOUND('',#1674,.T.);
#1177=FACE_OUTER_BOUND('',#1675,.T.);
#1178=FACE_OUTER_BOUND('',#1676,.T.);
#1179=FACE_OUTER_BOUND('',#1678,.T.);
#1180=FACE_OUTER_BOUND('',#1679,.T.);
#1181=FACE_OUTER_BOUND('',#1680,.T.);
#1182=FACE_OUTER_BOUND('',#1681,.T.);
#1183=FACE_OUTER_BOUND('',#1683,.T.);
#1184=FACE_OUTER_BOUND('',#1684,.T.);
#1185=FACE_OUTER_BOUND('',#1685,.T.);
#1186=FACE_OUTER_BOUND('',#1686,.T.);
#1187=FACE_OUTER_BOUND('',#1687,.T.);
#1188=FACE_OUTER_BOUND('',#1688,.T.);
#1189=FACE_OUTER_BOUND('',#1689,.T.);
#1190=FACE_OUTER_BOUND('',#1690,.T.);
#1191=FACE_OUTER_BOUND('',#1691,.T.);
#1192=FACE_OUTER_BOUND('',#1692,.T.);
#1193=FACE_OUTER_BOUND('',#1693,.T.);
#1194=FACE_OUTER_BOUND('',#1694,.T.);
#1195=FACE_OUTER_BOUND('',#1695,.T.);
#1196=FACE_OUTER_BOUND('',#1696,.T.);
#1197=FACE_OUTER_BOUND('',#1697,.T.);
#1198=FACE_OUTER_BOUND('',#1698,.T.);
#1199=FACE_OUTER_BOUND('',#1699,.T.);
#1200=FACE_OUTER_BOUND('',#1700,.T.);
#1201=FACE_OUTER_BOUND('',#1701,.T.);
#1202=FACE_OUTER_BOUND('',#1702,.T.);
#1203=FACE_OUTER_BOUND('',#1703,.T.);
#1204=FACE_OUTER_BOUND('',#1704,.T.);
#1205=FACE_OUTER_BOUND('',#1706,.T.);
#1206=FACE_OUTER_BOUND('',#1707,.T.);
#1207=FACE_OUTER_BOUND('',#1708,.T.);
#1208=FACE_OUTER_BOUND('',#1709,.T.);
#1209=FACE_OUTER_BOUND('',#1710,.T.);
#1210=FACE_OUTER_BOUND('',#1711,.T.);
#1211=FACE_OUTER_BOUND('',#1716,.T.);
#1212=FACE_OUTER_BOUND('',#1717,.T.);
#1213=FACE_OUTER_BOUND('',#1723,.T.);
#1214=FACE_OUTER_BOUND('',#1724,.T.);
#1215=FACE_OUTER_BOUND('',#1726,.T.);
#1216=FACE_OUTER_BOUND('',#1729,.T.);
#1217=FACE_OUTER_BOUND('',#1730,.T.);
#1218=FACE_OUTER_BOUND('',#1732,.T.);
#1219=FACE_OUTER_BOUND('',#1734,.T.);
#1220=FACE_OUTER_BOUND('',#1735,.T.);
#1221=FACE_OUTER_BOUND('',#1736,.T.);
#1222=FACE_OUTER_BOUND('',#1738,.T.);
#1223=FACE_OUTER_BOUND('',#1740,.T.);
#1224=FACE_OUTER_BOUND('',#1741,.T.);
#1225=FACE_OUTER_BOUND('',#1742,.T.);
#1226=FACE_OUTER_BOUND('',#1744,.T.);
#1227=FACE_OUTER_BOUND('',#1745,.T.);
#1228=FACE_OUTER_BOUND('',#1746,.T.);
#1229=FACE_OUTER_BOUND('',#1748,.T.);
#1230=FACE_OUTER_BOUND('',#1749,.T.);
#1231=FACE_OUTER_BOUND('',#1750,.T.);
#1232=FACE_OUTER_BOUND('',#1752,.T.);
#1233=FACE_OUTER_BOUND('',#1753,.T.);
#1234=FACE_OUTER_BOUND('',#1754,.T.);
#1235=FACE_OUTER_BOUND('',#1756,.T.);
#1236=FACE_OUTER_BOUND('',#1757,.T.);
#1237=FACE_OUTER_BOUND('',#1758,.T.);
#1238=FACE_OUTER_BOUND('',#1759,.T.);
#1239=FACE_OUTER_BOUND('',#1760,.T.);
#1240=FACE_OUTER_BOUND('',#1761,.T.);
#1241=FACE_OUTER_BOUND('',#1762,.T.);
#1242=FACE_OUTER_BOUND('',#1763,.T.);
#1243=FACE_OUTER_BOUND('',#1764,.T.);
#1244=FACE_OUTER_BOUND('',#1765,.T.);
#1245=FACE_OUTER_BOUND('',#1767,.T.);
#1246=FACE_OUTER_BOUND('',#1768,.T.);
#1247=FACE_OUTER_BOUND('',#1769,.T.);
#1248=FACE_OUTER_BOUND('',#1770,.T.);
#1249=FACE_OUTER_BOUND('',#1772,.T.);
#1250=FACE_OUTER_BOUND('',#1773,.T.);
#1251=FACE_OUTER_BOUND('',#1774,.T.);
#1252=FACE_OUTER_BOUND('',#1775,.T.);
#1253=FACE_OUTER_BOUND('',#1776,.T.);
#1254=FACE_OUTER_BOUND('',#1778,.T.);
#1255=FACE_OUTER_BOUND('',#1780,.T.);
#1256=FACE_OUTER_BOUND('',#1781,.T.);
#1257=FACE_OUTER_BOUND('',#1782,.T.);
#1258=FACE_OUTER_BOUND('',#1784,.T.);
#1259=FACE_OUTER_BOUND('',#1786,.T.);
#1260=FACE_OUTER_BOUND('',#1787,.T.);
#1261=FACE_OUTER_BOUND('',#1788,.T.);
#1262=FACE_OUTER_BOUND('',#1790,.T.);
#1263=FACE_OUTER_BOUND('',#1792,.T.);
#1264=FACE_OUTER_BOUND('',#1793,.T.);
#1265=FACE_OUTER_BOUND('',#1795,.T.);
#1266=FACE_OUTER_BOUND('',#1796,.T.);
#1267=FACE_OUTER_BOUND('',#1798,.T.);
#1268=FACE_OUTER_BOUND('',#1799,.T.);
#1269=FACE_OUTER_BOUND('',#1800,.T.);
#1270=FACE_OUTER_BOUND('',#1801,.T.);
#1271=FACE_OUTER_BOUND('',#1803,.T.);
#1272=FACE_OUTER_BOUND('',#1804,.T.);
#1273=FACE_OUTER_BOUND('',#1806,.T.);
#1274=FACE_OUTER_BOUND('',#1807,.T.);
#1275=FACE_OUTER_BOUND('',#1808,.T.);
#1276=FACE_OUTER_BOUND('',#1809,.T.);
#1277=FACE_OUTER_BOUND('',#1810,.T.);
#1278=FACE_OUTER_BOUND('',#1811,.T.);
#1279=FACE_OUTER_BOUND('',#1812,.T.);
#1280=FACE_OUTER_BOUND('',#1817,.T.);
#1281=FACE_OUTER_BOUND('',#1822,.T.);
#1282=FACE_OUTER_BOUND('',#1823,.T.);
#1283=FACE_OUTER_BOUND('',#1824,.T.);
#1284=FACE_OUTER_BOUND('',#1825,.T.);
#1285=FACE_OUTER_BOUND('',#1826,.T.);
#1286=FACE_OUTER_BOUND('',#1828,.T.);
#1287=FACE_OUTER_BOUND('',#1829,.T.);
#1288=FACE_OUTER_BOUND('',#1830,.T.);
#1289=FACE_OUTER_BOUND('',#1831,.T.);
#1290=FACE_OUTER_BOUND('',#1832,.T.);
#1291=FACE_OUTER_BOUND('',#1833,.T.);
#1292=FACE_OUTER_BOUND('',#1834,.T.);
#1293=FACE_OUTER_BOUND('',#1835,.T.);
#1294=FACE_OUTER_BOUND('',#1836,.T.);
#1295=FACE_OUTER_BOUND('',#1837,.T.);
#1296=FACE_OUTER_BOUND('',#1838,.T.);
#1297=FACE_OUTER_BOUND('',#1839,.T.);
#1298=FACE_OUTER_BOUND('',#1840,.T.);
#1299=FACE_OUTER_BOUND('',#1841,.T.);
#1300=FACE_OUTER_BOUND('',#1843,.T.);
#1301=FACE_OUTER_BOUND('',#1845,.T.);
#1302=FACE_OUTER_BOUND('',#1847,.T.);
#1303=FACE_OUTER_BOUND('',#1848,.T.);
#1304=FACE_OUTER_BOUND('',#1849,.T.);
#1305=FACE_OUTER_BOUND('',#1850,.T.);
#1306=FACE_OUTER_BOUND('',#1851,.T.);
#1307=FACE_OUTER_BOUND('',#1852,.T.);
#1308=FACE_OUTER_BOUND('',#1853,.T.);
#1309=FACE_OUTER_BOUND('',#1855,.T.);
#1310=FACE_OUTER_BOUND('',#1856,.T.);
#1311=FACE_OUTER_BOUND('',#1858,.T.);
#1312=FACE_OUTER_BOUND('',#1859,.T.);
#1313=FACE_OUTER_BOUND('',#1860,.T.);
#1314=FACE_OUTER_BOUND('',#1862,.T.);
#1315=FACE_OUTER_BOUND('',#1863,.T.);
#1316=FACE_OUTER_BOUND('',#1865,.T.);
#1317=FACE_OUTER_BOUND('',#1866,.T.);
#1318=FACE_OUTER_BOUND('',#1868,.T.);
#1319=FACE_OUTER_BOUND('',#1869,.T.);
#1320=FACE_OUTER_BOUND('',#1871,.T.);
#1321=FACE_OUTER_BOUND('',#1872,.T.);
#1322=FACE_OUTER_BOUND('',#1873,.T.);
#1323=FACE_OUTER_BOUND('',#1874,.T.);
#1324=FACE_OUTER_BOUND('',#1876,.T.);
#1325=FACE_OUTER_BOUND('',#1878,.T.);
#1326=FACE_OUTER_BOUND('',#1879,.T.);
#1327=FACE_OUTER_BOUND('',#1880,.T.);
#1328=FACE_OUTER_BOUND('',#1881,.T.);
#1329=FACE_OUTER_BOUND('',#1883,.T.);
#1330=FACE_OUTER_BOUND('',#1885,.T.);
#1331=FACE_OUTER_BOUND('',#1886,.T.);
#1332=FACE_OUTER_BOUND('',#1887,.T.);
#1333=FACE_OUTER_BOUND('',#1888,.T.);
#1334=FACE_OUTER_BOUND('',#1889,.T.);
#1335=FACE_OUTER_BOUND('',#1890,.T.);
#1336=FACE_OUTER_BOUND('',#1891,.T.);
#1337=FACE_OUTER_BOUND('',#1893,.T.);
#1338=FACE_OUTER_BOUND('',#1894,.T.);
#1339=FACE_OUTER_BOUND('',#1896,.T.);
#1340=FACE_OUTER_BOUND('',#1897,.T.);
#1341=FACE_OUTER_BOUND('',#1898,.T.);
#1342=FACE_OUTER_BOUND('',#1899,.T.);
#1343=FACE_OUTER_BOUND('',#1900,.T.);
#1344=FACE_OUTER_BOUND('',#1901,.T.);
#1345=FACE_OUTER_BOUND('',#1902,.T.);
#1346=FACE_OUTER_BOUND('',#1903,.T.);
#1347=FACE_OUTER_BOUND('',#1904,.T.);
#1348=FACE_OUTER_BOUND('',#1905,.T.);
#1349=FACE_OUTER_BOUND('',#1907,.T.);
#1350=FACE_OUTER_BOUND('',#1909,.T.);
#1351=FACE_OUTER_BOUND('',#1910,.T.);
#1352=FACE_OUTER_BOUND('',#1911,.T.);
#1353=FACE_OUTER_BOUND('',#1912,.T.);
#1354=FACE_OUTER_BOUND('',#1913,.T.);
#1355=FACE_OUTER_BOUND('',#1914,.T.);
#1356=FACE_OUTER_BOUND('',#1915,.T.);
#1357=FACE_OUTER_BOUND('',#1916,.T.);
#1358=FACE_OUTER_BOUND('',#1917,.T.);
#1359=FACE_OUTER_BOUND('',#1918,.T.);
#1360=FACE_OUTER_BOUND('',#1919,.T.);
#1361=FACE_OUTER_BOUND('',#1920,.T.);
#1362=FACE_OUTER_BOUND('',#1921,.T.);
#1363=FACE_OUTER_BOUND('',#1922,.T.);
#1364=FACE_OUTER_BOUND('',#1923,.T.);
#1365=FACE_OUTER_BOUND('',#1924,.T.);
#1366=FACE_OUTER_BOUND('',#1925,.T.);
#1367=FACE_OUTER_BOUND('',#1931,.T.);
#1368=FACE_OUTER_BOUND('',#1937,.T.);
#1369=FACE_OUTER_BOUND('',#1938,.T.);
#1370=FACE_OUTER_BOUND('',#1939,.T.);
#1371=FACE_OUTER_BOUND('',#1940,.T.);
#1372=FACE_OUTER_BOUND('',#1941,.T.);
#1373=FACE_OUTER_BOUND('',#1942,.T.);
#1374=FACE_OUTER_BOUND('',#1943,.T.);
#1375=FACE_OUTER_BOUND('',#1944,.T.);
#1376=FACE_OUTER_BOUND('',#1945,.T.);
#1377=FACE_OUTER_BOUND('',#1951,.T.);
#1378=FACE_OUTER_BOUND('',#1957,.T.);
#1379=FACE_OUTER_BOUND('',#1958,.T.);
#1380=FACE_OUTER_BOUND('',#1959,.T.);
#1381=FACE_OUTER_BOUND('',#1960,.T.);
#1382=FACE_OUTER_BOUND('',#1961,.T.);
#1383=FACE_OUTER_BOUND('',#1972,.T.);
#1384=FACE_OUTER_BOUND('',#1981,.T.);
#1385=FACE_OUTER_BOUND('',#1982,.T.);
#1386=FACE_OUTER_BOUND('',#1983,.T.);
#1387=FACE_OUTER_BOUND('',#1984,.T.);
#1388=FACE_OUTER_BOUND('',#1985,.T.);
#1389=FACE_OUTER_BOUND('',#1986,.T.);
#1390=FACE_OUTER_BOUND('',#1987,.T.);
#1391=FACE_OUTER_BOUND('',#1993,.T.);
#1392=FACE_OUTER_BOUND('',#1999,.T.);
#1393=FACE_OUTER_BOUND('',#2000,.T.);
#1394=FACE_OUTER_BOUND('',#2001,.T.);
#1395=FACE_OUTER_BOUND('',#2002,.T.);
#1396=FACE_OUTER_BOUND('',#2003,.T.);
#1397=FACE_OUTER_BOUND('',#2004,.T.);
#1398=FACE_OUTER_BOUND('',#2005,.T.);
#1399=FACE_OUTER_BOUND('',#2011,.T.);
#1400=FACE_OUTER_BOUND('',#2017,.T.);
#1401=FACE_OUTER_BOUND('',#2018,.T.);
#1402=FACE_OUTER_BOUND('',#2019,.T.);
#1403=FACE_OUTER_BOUND('',#2020,.T.);
#1404=FACE_OUTER_BOUND('',#2021,.T.);
#1405=FACE_OUTER_BOUND('',#2022,.T.);
#1406=FACE_OUTER_BOUND('',#2023,.T.);
#1407=FACE_OUTER_BOUND('',#2029,.T.);
#1408=FACE_OUTER_BOUND('',#2035,.T.);
#1409=FACE_OUTER_BOUND('',#2036,.T.);
#1410=FACE_OUTER_BOUND('',#2037,.T.);
#1411=FACE_OUTER_BOUND('',#2038,.T.);
#1412=FACE_OUTER_BOUND('',#2039,.T.);
#1413=FACE_OUTER_BOUND('',#2040,.T.);
#1414=FACE_OUTER_BOUND('',#2041,.T.);
#1415=FACE_OUTER_BOUND('',#2047,.T.);
#1416=FACE_OUTER_BOUND('',#2053,.T.);
#1417=FACE_OUTER_BOUND('',#2054,.T.);
#1418=FACE_OUTER_BOUND('',#2055,.T.);
#1419=FACE_OUTER_BOUND('',#2056,.T.);
#1420=FACE_OUTER_BOUND('',#2057,.T.);
#1421=FACE_OUTER_BOUND('',#2058,.T.);
#1422=FACE_OUTER_BOUND('',#2060,.T.);
#1423=FACE_OUTER_BOUND('',#2061,.T.);
#1424=FACE_OUTER_BOUND('',#2063,.T.);
#1425=FACE_OUTER_BOUND('',#2064,.T.);
#1426=FACE_OUTER_BOUND('',#2066,.T.);
#1427=FACE_OUTER_BOUND('',#2067,.T.);
#1428=FACE_OUTER_BOUND('',#2069,.T.);
#1429=FACE_OUTER_BOUND('',#2070,.T.);
#1430=FACE_OUTER_BOUND('',#2072,.T.);
#1431=FACE_OUTER_BOUND('',#2073,.T.);
#1432=FACE_OUTER_BOUND('',#2075,.T.);
#1433=FACE_OUTER_BOUND('',#2077,.T.);
#1434=FACE_OUTER_BOUND('',#2078,.T.);
#1435=FACE_OUTER_BOUND('',#2079,.T.);
#1436=FACE_OUTER_BOUND('',#2080,.T.);
#1437=FACE_OUTER_BOUND('',#2081,.T.);
#1438=FACE_OUTER_BOUND('',#2083,.T.);
#1439=FACE_OUTER_BOUND('',#2085,.T.);
#1440=FACE_OUTER_BOUND('',#2087,.T.);
#1441=FACE_OUTER_BOUND('',#2089,.T.);
#1442=FACE_OUTER_BOUND('',#2090,.T.);
#1443=FACE_OUTER_BOUND('',#2091,.T.);
#1444=FACE_OUTER_BOUND('',#2092,.T.);
#1445=FACE_OUTER_BOUND('',#2093,.T.);
#1446=FACE_OUTER_BOUND('',#2094,.T.);
#1447=FACE_OUTER_BOUND('',#2095,.T.);
#1448=FACE_OUTER_BOUND('',#2096,.T.);
#1449=FACE_OUTER_BOUND('',#2097,.T.);
#1450=FACE_OUTER_BOUND('',#2098,.T.);
#1451=FACE_OUTER_BOUND('',#2099,.T.);
#1452=FACE_OUTER_BOUND('',#2100,.T.);
#1453=FACE_OUTER_BOUND('',#2101,.T.);
#1454=FACE_OUTER_BOUND('',#2102,.T.);
#1455=FACE_OUTER_BOUND('',#2104,.T.);
#1456=FACE_OUTER_BOUND('',#2105,.T.);
#1457=FACE_OUTER_BOUND('',#2106,.T.);
#1458=FACE_OUTER_BOUND('',#2107,.T.);
#1459=FACE_OUTER_BOUND('',#2108,.T.);
#1460=FACE_OUTER_BOUND('',#2109,.T.);
#1461=FACE_OUTER_BOUND('',#2110,.T.);
#1462=FACE_OUTER_BOUND('',#2111,.T.);
#1463=FACE_OUTER_BOUND('',#2112,.T.);
#1464=FACE_OUTER_BOUND('',#2113,.T.);
#1465=FACE_OUTER_BOUND('',#2114,.T.);
#1466=FACE_OUTER_BOUND('',#2116,.T.);
#1467=FACE_OUTER_BOUND('',#2117,.T.);
#1468=FACE_OUTER_BOUND('',#2118,.T.);
#1469=FACE_OUTER_BOUND('',#2119,.T.);
#1470=FACE_OUTER_BOUND('',#2120,.T.);
#1471=FACE_OUTER_BOUND('',#2121,.T.);
#1472=FACE_OUTER_BOUND('',#2122,.T.);
#1473=FACE_OUTER_BOUND('',#2124,.T.);
#1474=FACE_OUTER_BOUND('',#2125,.T.);
#1475=FACE_OUTER_BOUND('',#2126,.T.);
#1476=FACE_OUTER_BOUND('',#2127,.T.);
#1477=FACE_OUTER_BOUND('',#2128,.T.);
#1478=FACE_OUTER_BOUND('',#2130,.T.);
#1479=FACE_OUTER_BOUND('',#2131,.T.);
#1480=FACE_OUTER_BOUND('',#2133,.T.);
#1481=FACE_OUTER_BOUND('',#2135,.T.);
#1482=FACE_OUTER_BOUND('',#2136,.T.);
#1483=FACE_OUTER_BOUND('',#2137,.T.);
#1484=FACE_OUTER_BOUND('',#2138,.T.);
#1485=FACE_OUTER_BOUND('',#2140,.T.);
#1486=FACE_OUTER_BOUND('',#2142,.T.);
#1487=FACE_OUTER_BOUND('',#2143,.T.);
#1488=FACE_OUTER_BOUND('',#2144,.T.);
#1489=FACE_OUTER_BOUND('',#2145,.T.);
#1490=FACE_OUTER_BOUND('',#2146,.T.);
#1491=FACE_OUTER_BOUND('',#2148,.T.);
#1492=FACE_OUTER_BOUND('',#2149,.T.);
#1493=FACE_OUTER_BOUND('',#2150,.T.);
#1494=FACE_OUTER_BOUND('',#2151,.T.);
#1495=FACE_OUTER_BOUND('',#2152,.T.);
#1496=FACE_OUTER_BOUND('',#2153,.T.);
#1497=FACE_OUTER_BOUND('',#2155,.T.);
#1498=FACE_OUTER_BOUND('',#2156,.T.);
#1499=FACE_OUTER_BOUND('',#2157,.T.);
#1500=FACE_OUTER_BOUND('',#2158,.T.);
#1501=FACE_OUTER_BOUND('',#2159,.T.);
#1502=FACE_OUTER_BOUND('',#2160,.T.);
#1503=FACE_OUTER_BOUND('',#2161,.T.);
#1504=FACE_OUTER_BOUND('',#2162,.T.);
#1505=FACE_OUTER_BOUND('',#2163,.T.);
#1506=FACE_OUTER_BOUND('',#2164,.T.);
#1507=FACE_OUTER_BOUND('',#2165,.T.);
#1508=FACE_OUTER_BOUND('',#2166,.T.);
#1509=FACE_OUTER_BOUND('',#2167,.T.);
#1510=FACE_OUTER_BOUND('',#2168,.T.);
#1511=FACE_OUTER_BOUND('',#2169,.T.);
#1512=FACE_OUTER_BOUND('',#2170,.T.);
#1513=FACE_OUTER_BOUND('',#2171,.T.);
#1514=FACE_OUTER_BOUND('',#2172,.T.);
#1515=FACE_OUTER_BOUND('',#2174,.T.);
#1516=FACE_OUTER_BOUND('',#2176,.T.);
#1517=FACE_OUTER_BOUND('',#2178,.T.);
#1518=FACE_OUTER_BOUND('',#2180,.T.);
#1519=FACE_OUTER_BOUND('',#2181,.T.);
#1520=FACE_OUTER_BOUND('',#2182,.T.);
#1521=FACE_OUTER_BOUND('',#2183,.T.);
#1522=FACE_OUTER_BOUND('',#2185,.T.);
#1523=FACE_OUTER_BOUND('',#2187,.T.);
#1524=FACE_OUTER_BOUND('',#2189,.T.);
#1525=FACE_OUTER_BOUND('',#2191,.T.);
#1526=FACE_OUTER_BOUND('',#2192,.T.);
#1527=FACE_OUTER_BOUND('',#2193,.T.);
#1528=FACE_OUTER_BOUND('',#2194,.T.);
#1529=FACE_OUTER_BOUND('',#2195,.T.);
#1530=FACE_OUTER_BOUND('',#2196,.T.);
#1531=FACE_OUTER_BOUND('',#2197,.T.);
#1532=FACE_OUTER_BOUND('',#2198,.T.);
#1533=FACE_OUTER_BOUND('',#2200,.T.);
#1534=FACE_OUTER_BOUND('',#2201,.T.);
#1535=FACE_OUTER_BOUND('',#2202,.T.);
#1536=FACE_OUTER_BOUND('',#2203,.T.);
#1537=FACE_OUTER_BOUND('',#2204,.T.);
#1538=FACE_OUTER_BOUND('',#2205,.T.);
#1539=FACE_OUTER_BOUND('',#2206,.T.);
#1540=FACE_OUTER_BOUND('',#2207,.T.);
#1541=FACE_OUTER_BOUND('',#2208,.T.);
#1542=FACE_OUTER_BOUND('',#2210,.T.);
#1543=FACE_OUTER_BOUND('',#2212,.T.);
#1544=FACE_OUTER_BOUND('',#2213,.T.);
#1545=FACE_OUTER_BOUND('',#2214,.T.);
#1546=FACE_OUTER_BOUND('',#2215,.T.);
#1547=FACE_OUTER_BOUND('',#2216,.T.);
#1548=FACE_OUTER_BOUND('',#2218,.T.);
#1549=FACE_OUTER_BOUND('',#2220,.T.);
#1550=FACE_OUTER_BOUND('',#2222,.T.);
#1551=FACE_OUTER_BOUND('',#2223,.T.);
#1552=FACE_OUTER_BOUND('',#2224,.T.);
#1553=FACE_OUTER_BOUND('',#2225,.T.);
#1554=FACE_OUTER_BOUND('',#2226,.T.);
#1555=FACE_OUTER_BOUND('',#2227,.T.);
#1556=FACE_OUTER_BOUND('',#2228,.T.);
#1557=FACE_OUTER_BOUND('',#2229,.T.);
#1558=FACE_OUTER_BOUND('',#2230,.T.);
#1559=FACE_OUTER_BOUND('',#2232,.T.);
#1560=FACE_OUTER_BOUND('',#2233,.T.);
#1561=FACE_OUTER_BOUND('',#2234,.T.);
#1562=FACE_OUTER_BOUND('',#2235,.T.);
#1563=FACE_OUTER_BOUND('',#2236,.T.);
#1564=FACE_OUTER_BOUND('',#2238,.T.);
#1565=FACE_OUTER_BOUND('',#2239,.T.);
#1566=FACE_OUTER_BOUND('',#2240,.T.);
#1567=FACE_OUTER_BOUND('',#2241,.T.);
#1568=FACE_OUTER_BOUND('',#2242,.T.);
#1569=FACE_OUTER_BOUND('',#2244,.T.);
#1570=FACE_OUTER_BOUND('',#2245,.T.);
#1571=FACE_OUTER_BOUND('',#2247,.T.);
#1572=FACE_OUTER_BOUND('',#2248,.T.);
#1573=FACE_OUTER_BOUND('',#2252,.T.);
#1574=FACE_OUTER_BOUND('',#2253,.T.);
#1575=FACE_OUTER_BOUND('',#2256,.T.);
#1576=FACE_OUTER_BOUND('',#2257,.T.);
#1577=FACE_OUTER_BOUND('',#2258,.T.);
#1578=FACE_OUTER_BOUND('',#2259,.T.);
#1579=FACE_OUTER_BOUND('',#2260,.T.);
#1580=FACE_OUTER_BOUND('',#2261,.T.);
#1581=FACE_OUTER_BOUND('',#2263,.T.);
#1582=FACE_OUTER_BOUND('',#2265,.T.);
#1583=FACE_OUTER_BOUND('',#2266,.T.);
#1584=FACE_OUTER_BOUND('',#2267,.T.);
#1585=FACE_OUTER_BOUND('',#2268,.T.);
#1586=FACE_OUTER_BOUND('',#2269,.T.);
#1587=FACE_OUTER_BOUND('',#2270,.T.);
#1588=FACE_OUTER_BOUND('',#2271,.T.);
#1589=FACE_OUTER_BOUND('',#2272,.T.);
#1590=FACE_OUTER_BOUND('',#2273,.T.);
#1591=FACE_OUTER_BOUND('',#2274,.T.);
#1592=FACE_OUTER_BOUND('',#2276,.T.);
#1593=EDGE_LOOP('',(#5316,#5317,#5318,#5319));
#1594=EDGE_LOOP('',(#5320));
#1595=EDGE_LOOP('',(#5321,#5322,#5323,#5324));
#1596=EDGE_LOOP('',(#5325));
#1597=EDGE_LOOP('',(#5326,#5327));
#1598=EDGE_LOOP('',(#5328,#5329));
#1599=EDGE_LOOP('',(#5330,#5331,#5332));
#1600=EDGE_LOOP('',(#5333,#5334,#5335,#5336,#5337,#5338,#5339,#5340,#5341,
#5342,#5343,#5344,#5345));
#1601=EDGE_LOOP('',(#5346,#5347,#5348));
#1602=EDGE_LOOP('',(#5349,#5350));
#1603=EDGE_LOOP('',(#5351,#5352));
#1604=EDGE_LOOP('',(#5353,#5354));
#1605=EDGE_LOOP('',(#5355,#5356));
#1606=EDGE_LOOP('',(#5357,#5358,#5359));
#1607=EDGE_LOOP('',(#5360,#5361,#5362,#5363,#5364,#5365,#5366,#5367,#5368));
#1608=EDGE_LOOP('',(#5369,#5370,#5371));
#1609=EDGE_LOOP('',(#5372,#5373,#5374,#5375,#5376,#5377,#5378,#5379));
#1610=EDGE_LOOP('',(#5380,#5381));
#1611=EDGE_LOOP('',(#5382,#5383,#5384,#5385));
#1612=EDGE_LOOP('',(#5386));
#1613=EDGE_LOOP('',(#5387));
#1614=EDGE_LOOP('',(#5388,#5389,#5390,#5391));
#1615=EDGE_LOOP('',(#5392,#5393,#5394,#5395));
#1616=EDGE_LOOP('',(#5396,#5397,#5398,#5399));
#1617=EDGE_LOOP('',(#5400,#5401,#5402,#5403));
#1618=EDGE_LOOP('',(#5404,#5405,#5406,#5407));
#1619=EDGE_LOOP('',(#5408,#5409,#5410,#5411));
#1620=EDGE_LOOP('',(#5412));
#1621=EDGE_LOOP('',(#5413,#5414,#5415,#5416));
#1622=EDGE_LOOP('',(#5417));
#1623=EDGE_LOOP('',(#5418));
#1624=EDGE_LOOP('',(#5419));
#1625=EDGE_LOOP('',(#5420));
#1626=EDGE_LOOP('',(#5421));
#1627=EDGE_LOOP('',(#5422,#5423,#5424,#5425));
#1628=EDGE_LOOP('',(#5426,#5427,#5428,#5429));
#1629=EDGE_LOOP('',(#5430));
#1630=EDGE_LOOP('',(#5431));
#1631=EDGE_LOOP('',(#5432));
#1632=EDGE_LOOP('',(#5433));
#1633=EDGE_LOOP('',(#5434));
#1634=EDGE_LOOP('',(#5435,#5436,#5437,#5438));
#1635=EDGE_LOOP('',(#5439,#5440,#5441,#5442));
#1636=EDGE_LOOP('',(#5443));
#1637=EDGE_LOOP('',(#5444,#5445,#5446,#5447));
#1638=EDGE_LOOP('',(#5448));
#1639=EDGE_LOOP('',(#5449));
#1640=EDGE_LOOP('',(#5450,#5451,#5452,#5453));
#1641=EDGE_LOOP('',(#5454));
#1642=EDGE_LOOP('',(#5455,#5456,#5457,#5458));
#1643=EDGE_LOOP('',(#5459,#5460));
#1644=EDGE_LOOP('',(#5461));
#1645=EDGE_LOOP('',(#5462,#5463,#5464,#5465));
#1646=EDGE_LOOP('',(#5466,#5467,#5468,#5469));
#1647=EDGE_LOOP('',(#5470));
#1648=EDGE_LOOP('',(#5471));
#1649=EDGE_LOOP('',(#5472));
#1650=EDGE_LOOP('',(#5473));
#1651=EDGE_LOOP('',(#5474,#5475,#5476,#5477));
#1652=EDGE_LOOP('',(#5478,#5479,#5480,#5481));
#1653=EDGE_LOOP('',(#5482,#5483));
#1654=EDGE_LOOP('',(#5484));
#1655=EDGE_LOOP('',(#5485,#5486,#5487,#5488,#5489,#5490));
#1656=EDGE_LOOP('',(#5491,#5492,#5493,#5494));
#1657=EDGE_LOOP('',(#5495,#5496,#5497,#5498,#5499,#5500));
#1658=EDGE_LOOP('',(#5501));
#1659=EDGE_LOOP('',(#5502,#5503,#5504,#5505));
#1660=EDGE_LOOP('',(#5506,#5507,#5508,#5509,#5510,#5511));
#1661=EDGE_LOOP('',(#5512,#5513,#5514,#5515));
#1662=EDGE_LOOP('',(#5516));
#1663=EDGE_LOOP('',(#5517,#5518,#5519,#5520,#5521,#5522));
#1664=EDGE_LOOP('',(#5523,#5524,#5525));
#1665=EDGE_LOOP('',(#5526,#5527,#5528,#5529,#5530,#5531));
#1666=EDGE_LOOP('',(#5532));
#1667=EDGE_LOOP('',(#5533,#5534,#5535,#5536));
#1668=EDGE_LOOP('',(#5537,#5538,#5539,#5540,#5541));
#1669=EDGE_LOOP('',(#5542,#5543,#5544,#5545,#5546));
#1670=EDGE_LOOP('',(#5547,#5548,#5549,#5550));
#1671=EDGE_LOOP('',(#5551,#5552,#5553,#5554,#5555));
#1672=EDGE_LOOP('',(#5556,#5557,#5558,#5559,#5560));
#1673=EDGE_LOOP('',(#5561,#5562,#5563));
#1674=EDGE_LOOP('',(#5564,#5565,#5566,#5567));
#1675=EDGE_LOOP('',(#5568,#5569,#5570,#5571));
#1676=EDGE_LOOP('',(#5572));
#1677=EDGE_LOOP('',(#5573));
#1678=EDGE_LOOP('',(#5574,#5575,#5576));
#1679=EDGE_LOOP('',(#5577,#5578,#5579,#5580));
#1680=EDGE_LOOP('',(#5581,#5582,#5583,#5584));
#1681=EDGE_LOOP('',(#5585));
#1682=EDGE_LOOP('',(#5586));
#1683=EDGE_LOOP('',(#5587,#5588,#5589,#5590));
#1684=EDGE_LOOP('',(#5591));
#1685=EDGE_LOOP('',(#5592,#5593,#5594,#5595));
#1686=EDGE_LOOP('',(#5596));
#1687=EDGE_LOOP('',(#5597,#5598,#5599,#5600));
#1688=EDGE_LOOP('',(#5601));
#1689=EDGE_LOOP('',(#5602,#5603));
#1690=EDGE_LOOP('',(#5604,#5605));
#1691=EDGE_LOOP('',(#5606,#5607));
#1692=EDGE_LOOP('',(#5608,#5609,#5610,#5611,#5612,#5613,#5614,#5615,#5616,
#5617,#5618,#5619,#5620));
#1693=EDGE_LOOP('',(#5621,#5622,#5623));
#1694=EDGE_LOOP('',(#5624,#5625,#5626));
#1695=EDGE_LOOP('',(#5627,#5628));
#1696=EDGE_LOOP('',(#5629,#5630));
#1697=EDGE_LOOP('',(#5631,#5632));
#1698=EDGE_LOOP('',(#5633,#5634));
#1699=EDGE_LOOP('',(#5635,#5636,#5637));
#1700=EDGE_LOOP('',(#5638,#5639,#5640));
#1701=EDGE_LOOP('',(#5641,#5642,#5643,#5644,#5645,#5646,#5647,#5648,#5649));
#1702=EDGE_LOOP('',(#5650,#5651,#5652,#5653));
#1703=EDGE_LOOP('',(#5654,#5655,#5656,#5657));
#1704=EDGE_LOOP('',(#5658));
#1705=EDGE_LOOP('',(#5659));
#1706=EDGE_LOOP('',(#5660,#5661,#5662,#5663));
#1707=EDGE_LOOP('',(#5664,#5665,#5666,#5667));
#1708=EDGE_LOOP('',(#5668,#5669,#5670,#5671));
#1709=EDGE_LOOP('',(#5672,#5673,#5674,#5675));
#1710=EDGE_LOOP('',(#5676,#5677,#5678,#5679,#5680,#5681,#5682,#5683));
#1711=EDGE_LOOP('',(#5684,#5685,#5686,#5687));
#1712=EDGE_LOOP('',(#5688));
#1713=EDGE_LOOP('',(#5689));
#1714=EDGE_LOOP('',(#5690));
#1715=EDGE_LOOP('',(#5691));
#1716=EDGE_LOOP('',(#5692,#5693,#5694,#5695));
#1717=EDGE_LOOP('',(#5696,#5697,#5698,#5699));
#1718=EDGE_LOOP('',(#5700));
#1719=EDGE_LOOP('',(#5701));
#1720=EDGE_LOOP('',(#5702));
#1721=EDGE_LOOP('',(#5703));
#1722=EDGE_LOOP('',(#5704));
#1723=EDGE_LOOP('',(#5705,#5706,#5707,#5708));
#1724=EDGE_LOOP('',(#5709,#5710,#5711,#5712));
#1725=EDGE_LOOP('',(#5713));
#1726=EDGE_LOOP('',(#5714,#5715,#5716,#5717));
#1727=EDGE_LOOP('',(#5718));
#1728=EDGE_LOOP('',(#5719));
#1729=EDGE_LOOP('',(#5720,#5721,#5722,#5723));
#1730=EDGE_LOOP('',(#5724));
#1731=EDGE_LOOP('',(#5725,#5726,#5727,#5728));
#1732=EDGE_LOOP('',(#5729,#5730));
#1733=EDGE_LOOP('',(#5731));
#1734=EDGE_LOOP('',(#5732,#5733,#5734,#5735));
#1735=EDGE_LOOP('',(#5736,#5737,#5738,#5739));
#1736=EDGE_LOOP('',(#5740));
#1737=EDGE_LOOP('',(#5741));
#1738=EDGE_LOOP('',(#5742));
#1739=EDGE_LOOP('',(#5743));
#1740=EDGE_LOOP('',(#5744,#5745,#5746,#5747));
#1741=EDGE_LOOP('',(#5748,#5749,#5750,#5751));
#1742=EDGE_LOOP('',(#5752,#5753));
#1743=EDGE_LOOP('',(#5754));
#1744=EDGE_LOOP('',(#5755,#5756,#5757,#5758,#5759,#5760));
#1745=EDGE_LOOP('',(#5761,#5762,#5763,#5764));
#1746=EDGE_LOOP('',(#5765,#5766,#5767,#5768,#5769,#5770));
#1747=EDGE_LOOP('',(#5771));
#1748=EDGE_LOOP('',(#5772,#5773,#5774,#5775));
#1749=EDGE_LOOP('',(#5776,#5777,#5778,#5779,#5780,#5781));
#1750=EDGE_LOOP('',(#5782,#5783,#5784,#5785));
#1751=EDGE_LOOP('',(#5786));
#1752=EDGE_LOOP('',(#5787,#5788,#5789,#5790,#5791,#5792));
#1753=EDGE_LOOP('',(#5793,#5794,#5795));
#1754=EDGE_LOOP('',(#5796,#5797,#5798,#5799,#5800,#5801));
#1755=EDGE_LOOP('',(#5802));
#1756=EDGE_LOOP('',(#5803,#5804,#5805,#5806));
#1757=EDGE_LOOP('',(#5807,#5808,#5809,#5810,#5811));
#1758=EDGE_LOOP('',(#5812,#5813,#5814,#5815,#5816));
#1759=EDGE_LOOP('',(#5817,#5818,#5819,#5820));
#1760=EDGE_LOOP('',(#5821,#5822,#5823,#5824,#5825));
#1761=EDGE_LOOP('',(#5826,#5827,#5828,#5829,#5830));
#1762=EDGE_LOOP('',(#5831,#5832,#5833));
#1763=EDGE_LOOP('',(#5834,#5835,#5836,#5837));
#1764=EDGE_LOOP('',(#5838,#5839,#5840,#5841));
#1765=EDGE_LOOP('',(#5842));
#1766=EDGE_LOOP('',(#5843));
#1767=EDGE_LOOP('',(#5844,#5845,#5846));
#1768=EDGE_LOOP('',(#5847,#5848,#5849,#5850));
#1769=EDGE_LOOP('',(#5851,#5852,#5853,#5854));
#1770=EDGE_LOOP('',(#5855));
#1771=EDGE_LOOP('',(#5856));
#1772=EDGE_LOOP('',(#5857,#5858,#5859,#5860));
#1773=EDGE_LOOP('',(#5861));
#1774=EDGE_LOOP('',(#5862,#5863,#5864,#5865));
#1775=EDGE_LOOP('',(#5866,#5867,#5868,#5869));
#1776=EDGE_LOOP('',(#5870));
#1777=EDGE_LOOP('',(#5871));
#1778=EDGE_LOOP('',(#5872));
#1779=EDGE_LOOP('',(#5873));
#1780=EDGE_LOOP('',(#5874,#5875,#5876,#5877));
#1781=EDGE_LOOP('',(#5878,#5879,#5880,#5881));
#1782=EDGE_LOOP('',(#5882));
#1783=EDGE_LOOP('',(#5883));
#1784=EDGE_LOOP('',(#5884));
#1785=EDGE_LOOP('',(#5885));
#1786=EDGE_LOOP('',(#5886,#5887,#5888,#5889));
#1787=EDGE_LOOP('',(#5890,#5891,#5892,#5893));
#1788=EDGE_LOOP('',(#5894));
#1789=EDGE_LOOP('',(#5895));
#1790=EDGE_LOOP('',(#5896));
#1791=EDGE_LOOP('',(#5897));
#1792=EDGE_LOOP('',(#5898,#5899,#5900,#5901));
#1793=EDGE_LOOP('',(#5902));
#1794=EDGE_LOOP('',(#5903));
#1795=EDGE_LOOP('',(#5904,#5905,#5906,#5907));
#1796=EDGE_LOOP('',(#5908));
#1797=EDGE_LOOP('',(#5909));
#1798=EDGE_LOOP('',(#5910,#5911,#5912,#5913));
#1799=EDGE_LOOP('',(#5914,#5915,#5916,#5917));
#1800=EDGE_LOOP('',(#5918,#5919,#5920,#5921));
#1801=EDGE_LOOP('',(#5922));
#1802=EDGE_LOOP('',(#5923));
#1803=EDGE_LOOP('',(#5924,#5925,#5926,#5927));
#1804=EDGE_LOOP('',(#5928));
#1805=EDGE_LOOP('',(#5929));
#1806=EDGE_LOOP('',(#5930,#5931,#5932,#5933));
#1807=EDGE_LOOP('',(#5934,#5935,#5936,#5937));
#1808=EDGE_LOOP('',(#5938,#5939,#5940,#5941));
#1809=EDGE_LOOP('',(#5942,#5943,#5944,#5945));
#1810=EDGE_LOOP('',(#5946,#5947,#5948,#5949));
#1811=EDGE_LOOP('',(#5950,#5951,#5952,#5953));
#1812=EDGE_LOOP('',(#5954,#5955,#5956,#5957));
#1813=EDGE_LOOP('',(#5958));
#1814=EDGE_LOOP('',(#5959));
#1815=EDGE_LOOP('',(#5960));
#1816=EDGE_LOOP('',(#5961));
#1817=EDGE_LOOP('',(#5962,#5963,#5964,#5965));
#1818=EDGE_LOOP('',(#5966));
#1819=EDGE_LOOP('',(#5967));
#1820=EDGE_LOOP('',(#5968));
#1821=EDGE_LOOP('',(#5969));
#1822=EDGE_LOOP('',(#5970));
#1823=EDGE_LOOP('',(#5971,#5972,#5973,#5974));
#1824=EDGE_LOOP('',(#5975,#5976,#5977,#5978));
#1825=EDGE_LOOP('',(#5979,#5980,#5981,#5982));
#1826=EDGE_LOOP('',(#5983));
#1827=EDGE_LOOP('',(#5984));
#1828=EDGE_LOOP('',(#5985,#5986,#5987,#5988));
#1829=EDGE_LOOP('',(#5989,#5990,#5991,#5992));
#1830=EDGE_LOOP('',(#5993,#5994,#5995,#5996));
#1831=EDGE_LOOP('',(#5997));
#1832=EDGE_LOOP('',(#5998,#5999,#6000,#6001));
#1833=EDGE_LOOP('',(#6002,#6003,#6004,#6005));
#1834=EDGE_LOOP('',(#6006,#6007,#6008,#6009));
#1835=EDGE_LOOP('',(#6010,#6011,#6012,#6013));
#1836=EDGE_LOOP('',(#6014,#6015,#6016,#6017));
#1837=EDGE_LOOP('',(#6018,#6019,#6020,#6021));
#1838=EDGE_LOOP('',(#6022,#6023,#6024,#6025,#6026,#6027));
#1839=EDGE_LOOP('',(#6028,#6029,#6030,#6031,#6032,#6033));
#1840=EDGE_LOOP('',(#6034,#6035,#6036,#6037));
#1841=EDGE_LOOP('',(#6038));
#1842=EDGE_LOOP('',(#6039));
#1843=EDGE_LOOP('',(#6040,#6041,#6042,#6043,#6044,#6045));
#1844=EDGE_LOOP('',(#6046));
#1845=EDGE_LOOP('',(#6047,#6048,#6049,#6050,#6051,#6052));
#1846=EDGE_LOOP('',(#6053));
#1847=EDGE_LOOP('',(#6054,#6055,#6056,#6057));
#1848=EDGE_LOOP('',(#6058,#6059,#6060,#6061));
#1849=EDGE_LOOP('',(#6062,#6063,#6064,#6065));
#1850=EDGE_LOOP('',(#6066,#6067,#6068,#6069));
#1851=EDGE_LOOP('',(#6070,#6071,#6072,#6073));
#1852=EDGE_LOOP('',(#6074,#6075,#6076,#6077));
#1853=EDGE_LOOP('',(#6078));
#1854=EDGE_LOOP('',(#6079));
#1855=EDGE_LOOP('',(#6080,#6081,#6082,#6083));
#1856=EDGE_LOOP('',(#6084));
#1857=EDGE_LOOP('',(#6085));
#1858=EDGE_LOOP('',(#6086,#6087,#6088,#6089));
#1859=EDGE_LOOP('',(#6090,#6091,#6092,#6093));
#1860=EDGE_LOOP('',(#6094));
#1861=EDGE_LOOP('',(#6095));
#1862=EDGE_LOOP('',(#6096,#6097,#6098,#6099));
#1863=EDGE_LOOP('',(#6100));
#1864=EDGE_LOOP('',(#6101));
#1865=EDGE_LOOP('',(#6102,#6103,#6104,#6105));
#1866=EDGE_LOOP('',(#6106));
#1867=EDGE_LOOP('',(#6107));
#1868=EDGE_LOOP('',(#6108,#6109,#6110,#6111));
#1869=EDGE_LOOP('',(#6112));
#1870=EDGE_LOOP('',(#6113));
#1871=EDGE_LOOP('',(#6114,#6115,#6116,#6117));
#1872=EDGE_LOOP('',(#6118,#6119,#6120,#6121));
#1873=EDGE_LOOP('',(#6122,#6123,#6124,#6125));
#1874=EDGE_LOOP('',(#6126));
#1875=EDGE_LOOP('',(#6127));
#1876=EDGE_LOOP('',(#6128));
#1877=EDGE_LOOP('',(#6129));
#1878=EDGE_LOOP('',(#6130,#6131,#6132,#6133));
#1879=EDGE_LOOP('',(#6134,#6135,#6136,#6137));
#1880=EDGE_LOOP('',(#6138,#6139,#6140,#6141));
#1881=EDGE_LOOP('',(#6142));
#1882=EDGE_LOOP('',(#6143));
#1883=EDGE_LOOP('',(#6144));
#1884=EDGE_LOOP('',(#6145));
#1885=EDGE_LOOP('',(#6146,#6147,#6148,#6149));
#1886=EDGE_LOOP('',(#6150,#6151,#6152,#6153));
#1887=EDGE_LOOP('',(#6154));
#1888=EDGE_LOOP('',(#6155));
#1889=EDGE_LOOP('',(#6156,#6157,#6158,#6159));
#1890=EDGE_LOOP('',(#6160,#6161,#6162,#6163));
#1891=EDGE_LOOP('',(#6164));
#1892=EDGE_LOOP('',(#6165));
#1893=EDGE_LOOP('',(#6166,#6167,#6168,#6169));
#1894=EDGE_LOOP('',(#6170));
#1895=EDGE_LOOP('',(#6171));
#1896=EDGE_LOOP('',(#6172,#6173,#6174,#6175,#6176,#6177,#6178,#6179,#6180));
#1897=EDGE_LOOP('',(#6181,#6182,#6183,#6184,#6185,#6186,#6187,#6188,#6189));
#1898=EDGE_LOOP('',(#6190,#6191,#6192,#6193));
#1899=EDGE_LOOP('',(#6194,#6195,#6196,#6197));
#1900=EDGE_LOOP('',(#6198,#6199,#6200,#6201));
#1901=EDGE_LOOP('',(#6202,#6203,#6204,#6205));
#1902=EDGE_LOOP('',(#6206,#6207,#6208,#6209));
#1903=EDGE_LOOP('',(#6210,#6211,#6212,#6213));
#1904=EDGE_LOOP('',(#6214,#6215,#6216,#6217));
#1905=EDGE_LOOP('',(#6218));
#1906=EDGE_LOOP('',(#6219));
#1907=EDGE_LOOP('',(#6220));
#1908=EDGE_LOOP('',(#6221));
#1909=EDGE_LOOP('',(#6222,#6223,#6224,#6225));
#1910=EDGE_LOOP('',(#6226,#6227,#6228,#6229));
#1911=EDGE_LOOP('',(#6230,#6231,#6232,#6233));
#1912=EDGE_LOOP('',(#6234,#6235,#6236,#6237));
#1913=EDGE_LOOP('',(#6238,#6239,#6240,#6241));
#1914=EDGE_LOOP('',(#6242,#6243,#6244,#6245));
#1915=EDGE_LOOP('',(#6246,#6247,#6248,#6249));
#1916=EDGE_LOOP('',(#6250,#6251,#6252,#6253));
#1917=EDGE_LOOP('',(#6254,#6255,#6256,#6257));
#1918=EDGE_LOOP('',(#6258,#6259,#6260,#6261));
#1919=EDGE_LOOP('',(#6262,#6263,#6264,#6265));
#1920=EDGE_LOOP('',(#6266,#6267,#6268,#6269));
#1921=EDGE_LOOP('',(#6270,#6271,#6272,#6273));
#1922=EDGE_LOOP('',(#6274,#6275,#6276,#6277));
#1923=EDGE_LOOP('',(#6278,#6279,#6280,#6281));
#1924=EDGE_LOOP('',(#6282,#6283,#6284,#6285));
#1925=EDGE_LOOP('',(#6286,#6287,#6288,#6289));
#1926=EDGE_LOOP('',(#6290));
#1927=EDGE_LOOP('',(#6291));
#1928=EDGE_LOOP('',(#6292));
#1929=EDGE_LOOP('',(#6293));
#1930=EDGE_LOOP('',(#6294));
#1931=EDGE_LOOP('',(#6295,#6296,#6297,#6298));
#1932=EDGE_LOOP('',(#6299));
#1933=EDGE_LOOP('',(#6300));
#1934=EDGE_LOOP('',(#6301));
#1935=EDGE_LOOP('',(#6302));
#1936=EDGE_LOOP('',(#6303));
#1937=EDGE_LOOP('',(#6304,#6305,#6306,#6307));
#1938=EDGE_LOOP('',(#6308,#6309,#6310,#6311));
#1939=EDGE_LOOP('',(#6312,#6313,#6314,#6315));
#1940=EDGE_LOOP('',(#6316,#6317,#6318,#6319));
#1941=EDGE_LOOP('',(#6320,#6321,#6322,#6323));
#1942=EDGE_LOOP('',(#6324,#6325,#6326,#6327));
#1943=EDGE_LOOP('',(#6328,#6329,#6330,#6331));
#1944=EDGE_LOOP('',(#6332,#6333,#6334,#6335));
#1945=EDGE_LOOP('',(#6336,#6337,#6338,#6339));
#1946=EDGE_LOOP('',(#6340));
#1947=EDGE_LOOP('',(#6341));
#1948=EDGE_LOOP('',(#6342));
#1949=EDGE_LOOP('',(#6343));
#1950=EDGE_LOOP('',(#6344));
#1951=EDGE_LOOP('',(#6345,#6346,#6347,#6348));
#1952=EDGE_LOOP('',(#6349));
#1953=EDGE_LOOP('',(#6350));
#1954=EDGE_LOOP('',(#6351));
#1955=EDGE_LOOP('',(#6352));
#1956=EDGE_LOOP('',(#6353));
#1957=EDGE_LOOP('',(#6354,#6355,#6356,#6357));
#1958=EDGE_LOOP('',(#6358,#6359,#6360,#6361));
#1959=EDGE_LOOP('',(#6362,#6363,#6364,#6365));
#1960=EDGE_LOOP('',(#6366,#6367,#6368,#6369));
#1961=EDGE_LOOP('',(#6370,#6371,#6372,#6373));
#1962=EDGE_LOOP('',(#6374,#6375,#6376,#6377));
#1963=EDGE_LOOP('',(#6378,#6379,#6380,#6381));
#1964=EDGE_LOOP('',(#6382));
#1965=EDGE_LOOP('',(#6383));
#1966=EDGE_LOOP('',(#6384));
#1967=EDGE_LOOP('',(#6385));
#1968=EDGE_LOOP('',(#6386));
#1969=EDGE_LOOP('',(#6387));
#1970=EDGE_LOOP('',(#6388));
#1971=EDGE_LOOP('',(#6389));
#1972=EDGE_LOOP('',(#6390,#6391,#6392,#6393));
#1973=EDGE_LOOP('',(#6394));
#1974=EDGE_LOOP('',(#6395));
#1975=EDGE_LOOP('',(#6396));
#1976=EDGE_LOOP('',(#6397));
#1977=EDGE_LOOP('',(#6398));
#1978=EDGE_LOOP('',(#6399));
#1979=EDGE_LOOP('',(#6400));
#1980=EDGE_LOOP('',(#6401));
#1981=EDGE_LOOP('',(#6402,#6403,#6404,#6405));
#1982=EDGE_LOOP('',(#6406,#6407,#6408,#6409));
#1983=EDGE_LOOP('',(#6410,#6411,#6412,#6413));
#1984=EDGE_LOOP('',(#6414,#6415,#6416,#6417));
#1985=EDGE_LOOP('',(#6418,#6419,#6420,#6421));
#1986=EDGE_LOOP('',(#6422,#6423,#6424,#6425));
#1987=EDGE_LOOP('',(#6426));
#1988=EDGE_LOOP('',(#6427));
#1989=EDGE_LOOP('',(#6428));
#1990=EDGE_LOOP('',(#6429));
#1991=EDGE_LOOP('',(#6430));
#1992=EDGE_LOOP('',(#6431));
#1993=EDGE_LOOP('',(#6432));
#1994=EDGE_LOOP('',(#6433));
#1995=EDGE_LOOP('',(#6434));
#1996=EDGE_LOOP('',(#6435));
#1997=EDGE_LOOP('',(#6436));
#1998=EDGE_LOOP('',(#6437));
#1999=EDGE_LOOP('',(#6438,#6439,#6440,#6441));
#2000=EDGE_LOOP('',(#6442,#6443,#6444,#6445));
#2001=EDGE_LOOP('',(#6446,#6447,#6448,#6449));
#2002=EDGE_LOOP('',(#6450,#6451,#6452,#6453));
#2003=EDGE_LOOP('',(#6454,#6455,#6456,#6457));
#2004=EDGE_LOOP('',(#6458,#6459,#6460,#6461));
#2005=EDGE_LOOP('',(#6462));
#2006=EDGE_LOOP('',(#6463));
#2007=EDGE_LOOP('',(#6464));
#2008=EDGE_LOOP('',(#6465));
#2009=EDGE_LOOP('',(#6466));
#2010=EDGE_LOOP('',(#6467));
#2011=EDGE_LOOP('',(#6468));
#2012=EDGE_LOOP('',(#6469));
#2013=EDGE_LOOP('',(#6470));
#2014=EDGE_LOOP('',(#6471));
#2015=EDGE_LOOP('',(#6472));
#2016=EDGE_LOOP('',(#6473));
#2017=EDGE_LOOP('',(#6474,#6475,#6476,#6477));
#2018=EDGE_LOOP('',(#6478,#6479,#6480,#6481));
#2019=EDGE_LOOP('',(#6482,#6483,#6484,#6485));
#2020=EDGE_LOOP('',(#6486,#6487,#6488,#6489));
#2021=EDGE_LOOP('',(#6490,#6491,#6492,#6493));
#2022=EDGE_LOOP('',(#6494,#6495,#6496,#6497));
#2023=EDGE_LOOP('',(#6498));
#2024=EDGE_LOOP('',(#6499));
#2025=EDGE_LOOP('',(#6500));
#2026=EDGE_LOOP('',(#6501));
#2027=EDGE_LOOP('',(#6502));
#2028=EDGE_LOOP('',(#6503));
#2029=EDGE_LOOP('',(#6504));
#2030=EDGE_LOOP('',(#6505));
#2031=EDGE_LOOP('',(#6506));
#2032=EDGE_LOOP('',(#6507));
#2033=EDGE_LOOP('',(#6508));
#2034=EDGE_LOOP('',(#6509));
#2035=EDGE_LOOP('',(#6510,#6511,#6512,#6513));
#2036=EDGE_LOOP('',(#6514,#6515,#6516,#6517));
#2037=EDGE_LOOP('',(#6518,#6519,#6520,#6521));
#2038=EDGE_LOOP('',(#6522,#6523,#6524,#6525));
#2039=EDGE_LOOP('',(#6526,#6527,#6528,#6529));
#2040=EDGE_LOOP('',(#6530,#6531,#6532,#6533));
#2041=EDGE_LOOP('',(#6534));
#2042=EDGE_LOOP('',(#6535));
#2043=EDGE_LOOP('',(#6536));
#2044=EDGE_LOOP('',(#6537));
#2045=EDGE_LOOP('',(#6538));
#2046=EDGE_LOOP('',(#6539));
#2047=EDGE_LOOP('',(#6540));
#2048=EDGE_LOOP('',(#6541));
#2049=EDGE_LOOP('',(#6542));
#2050=EDGE_LOOP('',(#6543));
#2051=EDGE_LOOP('',(#6544));
#2052=EDGE_LOOP('',(#6545));
#2053=EDGE_LOOP('',(#6546,#6547,#6548,#6549));
#2054=EDGE_LOOP('',(#6550,#6551,#6552,#6553));
#2055=EDGE_LOOP('',(#6554,#6555,#6556,#6557));
#2056=EDGE_LOOP('',(#6558,#6559,#6560,#6561));
#2057=EDGE_LOOP('',(#6562,#6563,#6564,#6565));
#2058=EDGE_LOOP('',(#6566));
#2059=EDGE_LOOP('',(#6567));
#2060=EDGE_LOOP('',(#6568,#6569,#6570,#6571));
#2061=EDGE_LOOP('',(#6572));
#2062=EDGE_LOOP('',(#6573));
#2063=EDGE_LOOP('',(#6574,#6575,#6576,#6577));
#2064=EDGE_LOOP('',(#6578));
#2065=EDGE_LOOP('',(#6579));
#2066=EDGE_LOOP('',(#6580,#6581,#6582,#6583));
#2067=EDGE_LOOP('',(#6584));
#2068=EDGE_LOOP('',(#6585));
#2069=EDGE_LOOP('',(#6586,#6587,#6588,#6589));
#2070=EDGE_LOOP('',(#6590));
#2071=EDGE_LOOP('',(#6591));
#2072=EDGE_LOOP('',(#6592,#6593,#6594,#6595));
#2073=EDGE_LOOP('',(#6596));
#2074=EDGE_LOOP('',(#6597));
#2075=EDGE_LOOP('',(#6598,#6599,#6600,#6601));
#2076=EDGE_LOOP('',(#6602,#6603,#6604,#6605));
#2077=EDGE_LOOP('',(#6606,#6607,#6608,#6609));
#2078=EDGE_LOOP('',(#6610,#6611,#6612,#6613));
#2079=EDGE_LOOP('',(#6614,#6615,#6616,#6617));
#2080=EDGE_LOOP('',(#6618,#6619,#6620,#6621));
#2081=EDGE_LOOP('',(#6622));
#2082=EDGE_LOOP('',(#6623));
#2083=EDGE_LOOP('',(#6624,#6625,#6626,#6627));
#2084=EDGE_LOOP('',(#6628,#6629,#6630,#6631));
#2085=EDGE_LOOP('',(#6632));
#2086=EDGE_LOOP('',(#6633));
#2087=EDGE_LOOP('',(#6634,#6635,#6636,#6637));
#2088=EDGE_LOOP('',(#6638,#6639,#6640,#6641));
#2089=EDGE_LOOP('',(#6642,#6643,#6644,#6645));
#2090=EDGE_LOOP('',(#6646,#6647,#6648,#6649));
#2091=EDGE_LOOP('',(#6650,#6651,#6652,#6653));
#2092=EDGE_LOOP('',(#6654,#6655,#6656,#6657));
#2093=EDGE_LOOP('',(#6658,#6659,#6660,#6661));
#2094=EDGE_LOOP('',(#6662,#6663,#6664,#6665));
#2095=EDGE_LOOP('',(#6666,#6667,#6668,#6669,#6670,#6671));
#2096=EDGE_LOOP('',(#6672,#6673,#6674,#6675,#6676,#6677));
#2097=EDGE_LOOP('',(#6678));
#2098=EDGE_LOOP('',(#6679));
#2099=EDGE_LOOP('',(#6680,#6681,#6682,#6683));
#2100=EDGE_LOOP('',(#6684,#6685,#6686,#6687));
#2101=EDGE_LOOP('',(#6688,#6689,#6690,#6691));
#2102=EDGE_LOOP('',(#6692));
#2103=EDGE_LOOP('',(#6693));
#2104=EDGE_LOOP('',(#6694,#6695,#6696,#6697));
#2105=EDGE_LOOP('',(#6698,#6699,#6700,#6701));
#2106=EDGE_LOOP('',(#6702,#6703,#6704,#6705));
#2107=EDGE_LOOP('',(#6706,#6707,#6708,#6709));
#2108=EDGE_LOOP('',(#6710,#6711,#6712,#6713));
#2109=EDGE_LOOP('',(#6714,#6715,#6716,#6717));
#2110=EDGE_LOOP('',(#6718,#6719,#6720,#6721));
#2111=EDGE_LOOP('',(#6722,#6723,#6724,#6725));
#2112=EDGE_LOOP('',(#6726,#6727,#6728,#6729,#6730,#6731));
#2113=EDGE_LOOP('',(#6732,#6733,#6734,#6735,#6736,#6737));
#2114=EDGE_LOOP('',(#6738));
#2115=EDGE_LOOP('',(#6739));
#2116=EDGE_LOOP('',(#6740,#6741,#6742,#6743));
#2117=EDGE_LOOP('',(#6744));
#2118=EDGE_LOOP('',(#6745));
#2119=EDGE_LOOP('',(#6746,#6747,#6748,#6749));
#2120=EDGE_LOOP('',(#6750,#6751,#6752,#6753));
#2121=EDGE_LOOP('',(#6754,#6755,#6756,#6757));
#2122=EDGE_LOOP('',(#6758));
#2123=EDGE_LOOP('',(#6759));
#2124=EDGE_LOOP('',(#6760,#6761,#6762,#6763));
#2125=EDGE_LOOP('',(#6764,#6765,#6766,#6767));
#2126=EDGE_LOOP('',(#6768,#6769,#6770,#6771));
#2127=EDGE_LOOP('',(#6772,#6773,#6774,#6775));
#2128=EDGE_LOOP('',(#6776));
#2129=EDGE_LOOP('',(#6777));
#2130=EDGE_LOOP('',(#6778,#6779,#6780,#6781));
#2131=EDGE_LOOP('',(#6782));
#2132=EDGE_LOOP('',(#6783));
#2133=EDGE_LOOP('',(#6784));
#2134=EDGE_LOOP('',(#6785));
#2135=EDGE_LOOP('',(#6786,#6787,#6788,#6789));
#2136=EDGE_LOOP('',(#6790,#6791,#6792,#6793));
#2137=EDGE_LOOP('',(#6794,#6795,#6796,#6797));
#2138=EDGE_LOOP('',(#6798));
#2139=EDGE_LOOP('',(#6799));
#2140=EDGE_LOOP('',(#6800));
#2141=EDGE_LOOP('',(#6801));
#2142=EDGE_LOOP('',(#6802,#6803,#6804,#6805));
#2143=EDGE_LOOP('',(#6806,#6807,#6808,#6809));
#2144=EDGE_LOOP('',(#6810));
#2145=EDGE_LOOP('',(#6811,#6812,#6813,#6814));
#2146=EDGE_LOOP('',(#6815));
#2147=EDGE_LOOP('',(#6816));
#2148=EDGE_LOOP('',(#6817));
#2149=EDGE_LOOP('',(#6818));
#2150=EDGE_LOOP('',(#6819,#6820,#6821,#6822));
#2151=EDGE_LOOP('',(#6823,#6824,#6825,#6826));
#2152=EDGE_LOOP('',(#6827,#6828,#6829,#6830));
#2153=EDGE_LOOP('',(#6831));
#2154=EDGE_LOOP('',(#6832));
#2155=EDGE_LOOP('',(#6833,#6834,#6835,#6836));
#2156=EDGE_LOOP('',(#6837,#6838,#6839,#6840));
#2157=EDGE_LOOP('',(#6841,#6842,#6843,#6844));
#2158=EDGE_LOOP('',(#6845));
#2159=EDGE_LOOP('',(#6846,#6847,#6848,#6849));
#2160=EDGE_LOOP('',(#6850,#6851,#6852,#6853));
#2161=EDGE_LOOP('',(#6854,#6855,#6856,#6857));
#2162=EDGE_LOOP('',(#6858,#6859,#6860,#6861));
#2163=EDGE_LOOP('',(#6862,#6863,#6864,#6865));
#2164=EDGE_LOOP('',(#6866,#6867,#6868,#6869));
#2165=EDGE_LOOP('',(#6870,#6871,#6872,#6873,#6874,#6875));
#2166=EDGE_LOOP('',(#6876,#6877,#6878,#6879,#6880,#6881));
#2167=EDGE_LOOP('',(#6882,#6883,#6884,#6885));
#2168=EDGE_LOOP('',(#6886,#6887,#6888,#6889));
#2169=EDGE_LOOP('',(#6890,#6891));
#2170=EDGE_LOOP('',(#6892,#6893,#6894,#6895,#6896,#6897,#6898,#6899));
#2171=EDGE_LOOP('',(#6900,#6901,#6902));
#2172=EDGE_LOOP('',(#6903,#6904,#6905,#6906));
#2173=EDGE_LOOP('',(#6907,#6908,#6909,#6910));
#2174=EDGE_LOOP('',(#6911,#6912,#6913,#6914));
#2175=EDGE_LOOP('',(#6915));
#2176=EDGE_LOOP('',(#6916,#6917,#6918,#6919));
#2177=EDGE_LOOP('',(#6920));
#2178=EDGE_LOOP('',(#6921,#6922,#6923,#6924));
#2179=EDGE_LOOP('',(#6925));
#2180=EDGE_LOOP('',(#6926,#6927,#6928,#6929,#6930,#6931,#6932,#6933));
#2181=EDGE_LOOP('',(#6934,#6935,#6936,#6937));
#2182=EDGE_LOOP('',(#6938,#6939,#6940,#6941));
#2183=EDGE_LOOP('',(#6942,#6943,#6944,#6945));
#2184=EDGE_LOOP('',(#6946));
#2185=EDGE_LOOP('',(#6947,#6948,#6949,#6950));
#2186=EDGE_LOOP('',(#6951));
#2187=EDGE_LOOP('',(#6952,#6953,#6954,#6955));
#2188=EDGE_LOOP('',(#6956));
#2189=EDGE_LOOP('',(#6957,#6958,#6959,#6960,#6961,#6962,#6963,#6964));
#2190=EDGE_LOOP('',(#6965));
#2191=EDGE_LOOP('',(#6966,#6967,#6968,#6969));
#2192=EDGE_LOOP('',(#6970,#6971,#6972,#6973));
#2193=EDGE_LOOP('',(#6974,#6975,#6976,#6977));
#2194=EDGE_LOOP('',(#6978,#6979,#6980,#6981));
#2195=EDGE_LOOP('',(#6982,#6983,#6984,#6985));
#2196=EDGE_LOOP('',(#6986,#6987,#6988,#6989));
#2197=EDGE_LOOP('',(#6990,#6991,#6992,#6993,#6994,#6995));
#2198=EDGE_LOOP('',(#6996));
#2199=EDGE_LOOP('',(#6997,#6998,#6999,#7000,#7001,#7002));
#2200=EDGE_LOOP('',(#7003,#7004,#7005,#7006));
#2201=EDGE_LOOP('',(#7007,#7008,#7009,#7010));
#2202=EDGE_LOOP('',(#7011,#7012,#7013,#7014));
#2203=EDGE_LOOP('',(#7015));
#2204=EDGE_LOOP('',(#7016,#7017,#7018,#7019,#7020,#7021));
#2205=EDGE_LOOP('',(#7022));
#2206=EDGE_LOOP('',(#7023,#7024,#7025,#7026));
#2207=EDGE_LOOP('',(#7027,#7028,#7029,#7030));
#2208=EDGE_LOOP('',(#7031));
#2209=EDGE_LOOP('',(#7032));
#2210=EDGE_LOOP('',(#7033,#7034,#7035,#7036,#7037,#7038,#7039,#7040,#7041));
#2211=EDGE_LOOP('',(#7042));
#2212=EDGE_LOOP('',(#7043,#7044,#7045,#7046));
#2213=EDGE_LOOP('',(#7047));
#2214=EDGE_LOOP('',(#7048,#7049,#7050,#7051));
#2215=EDGE_LOOP('',(#7052,#7053,#7054,#7055));
#2216=EDGE_LOOP('',(#7056));
#2217=EDGE_LOOP('',(#7057));
#2218=EDGE_LOOP('',(#7058));
#2219=EDGE_LOOP('',(#7059));
#2220=EDGE_LOOP('',(#7060,#7061,#7062,#7063));
#2221=EDGE_LOOP('',(#7064,#7065));
#2222=EDGE_LOOP('',(#7066,#7067));
#2223=EDGE_LOOP('',(#7068,#7069,#7070,#7071));
#2224=EDGE_LOOP('',(#7072,#7073,#7074,#7075,#7076,#7077,#7078,#7079,#7080));
#2225=EDGE_LOOP('',(#7081,#7082,#7083));
#2226=EDGE_LOOP('',(#7084,#7085,#7086,#7087));
#2227=EDGE_LOOP('',(#7088));
#2228=EDGE_LOOP('',(#7089,#7090,#7091,#7092));
#2229=EDGE_LOOP('',(#7093));
#2230=EDGE_LOOP('',(#7094));
#2231=EDGE_LOOP('',(#7095));
#2232=EDGE_LOOP('',(#7096,#7097,#7098,#7099));
#2233=EDGE_LOOP('',(#7100));
#2234=EDGE_LOOP('',(#7101,#7102,#7103,#7104));
#2235=EDGE_LOOP('',(#7105));
#2236=EDGE_LOOP('',(#7106));
#2237=EDGE_LOOP('',(#7107));
#2238=EDGE_LOOP('',(#7108,#7109,#7110,#7111));
#2239=EDGE_LOOP('',(#7112,#7113,#7114,#7115));
#2240=EDGE_LOOP('',(#7116,#7117,#7118,#7119));
#2241=EDGE_LOOP('',(#7120,#7121,#7122,#7123));
#2242=EDGE_LOOP('',(#7124,#7125,#7126,#7127));
#2243=EDGE_LOOP('',(#7128));
#2244=EDGE_LOOP('',(#7129,#7130,#7131,#7132));
#2245=EDGE_LOOP('',(#7133,#7134,#7135,#7136));
#2246=EDGE_LOOP('',(#7137));
#2247=EDGE_LOOP('',(#7138,#7139,#7140,#7141));
#2248=EDGE_LOOP('',(#7142,#7143,#7144,#7145));
#2249=EDGE_LOOP('',(#7146));
#2250=EDGE_LOOP('',(#7147));
#2251=EDGE_LOOP('',(#7148,#7149,#7150,#7151));
#2252=EDGE_LOOP('',(#7152,#7153,#7154,#7155));
#2253=EDGE_LOOP('',(#7156,#7157,#7158,#7159));
#2254=EDGE_LOOP('',(#7160));
#2255=EDGE_LOOP('',(#7161));
#2256=EDGE_LOOP('',(#7162,#7163,#7164,#7165));
#2257=EDGE_LOOP('',(#7166,#7167,#7168,#7169));
#2258=EDGE_LOOP('',(#7170,#7171,#7172,#7173));
#2259=EDGE_LOOP('',(#7174,#7175,#7176,#7177));
#2260=EDGE_LOOP('',(#7178,#7179,#7180,#7181));
#2261=EDGE_LOOP('',(#7182));
#2262=EDGE_LOOP('',(#7183));
#2263=EDGE_LOOP('',(#7184));
#2264=EDGE_LOOP('',(#7185));
#2265=EDGE_LOOP('',(#7186,#7187,#7188,#7189,#7190,#7191,#7192,#7193,#7194));
#2266=EDGE_LOOP('',(#7195,#7196,#7197,#7198,#7199,#7200,#7201,#7202,#7203));
#2267=EDGE_LOOP('',(#7204,#7205,#7206,#7207));
#2268=EDGE_LOOP('',(#7208,#7209,#7210,#7211));
#2269=EDGE_LOOP('',(#7212,#7213,#7214,#7215));
#2270=EDGE_LOOP('',(#7216,#7217,#7218,#7219));
#2271=EDGE_LOOP('',(#7220,#7221,#7222,#7223));
#2272=EDGE_LOOP('',(#7224,#7225,#7226,#7227));
#2273=EDGE_LOOP('',(#7228,#7229,#7230,#7231));
#2274=EDGE_LOOP('',(#7232));
#2275=EDGE_LOOP('',(#7233));
#2276=EDGE_LOOP('',(#7234));
#2277=EDGE_LOOP('',(#7235));
#2278=LINE('',#11927,#2823);
#2279=LINE('',#11934,#2824);
#2280=LINE('',#11940,#2825);
#2281=LINE('',#11944,#2826);
#2282=LINE('',#11952,#2827);
#2283=LINE('',#11954,#2828);
#2284=LINE('',#11959,#2829);
#2285=LINE('',#11963,#2830);
#2286=LINE('',#11967,#2831);
#2287=LINE('',#11978,#2832);
#2288=LINE('',#11986,#2833);
#2289=LINE('',#11994,#2834);
#2290=LINE('',#12002,#2835);
#2291=LINE('',#12009,#2836);
#2292=LINE('',#12015,#2837);
#2293=LINE('',#12021,#2838);
#2294=LINE('',#12027,#2839);
#2295=LINE('',#12033,#2840);
#2296=LINE('',#12039,#2841);
#2297=LINE('',#12041,#2842);
#2298=LINE('',#12043,#2843);
#2299=LINE('',#12044,#2844);
#2300=LINE('',#12047,#2845);
#2301=LINE('',#12049,#2846);
#2302=LINE('',#12050,#2847);
#2303=LINE('',#12053,#2848);
#2304=LINE('',#12055,#2849);
#2305=LINE('',#12056,#2850);
#2306=LINE('',#12058,#2851);
#2307=LINE('',#12059,#2852);
#2308=LINE('',#12067,#2853);
#2309=LINE('',#12072,#2854);
#2310=LINE('',#12074,#2855);
#2311=LINE('',#12076,#2856);
#2312=LINE('',#12077,#2857);
#2313=LINE('',#12088,#2858);
#2314=LINE('',#12097,#2859);
#2315=LINE('',#12100,#2860);
#2316=LINE('',#12108,#2861);
#2317=LINE('',#12110,#2862);
#2318=LINE('',#12112,#2863);
#2319=LINE('',#12114,#2864);
#2320=LINE('',#12116,#2865);
#2321=LINE('',#12117,#2866);
#2322=LINE('',#12121,#2867);
#2323=LINE('',#12123,#2868);
#2324=LINE('',#12125,#2869);
#2325=LINE('',#12126,#2870);
#2326=LINE('',#12129,#2871);
#2327=LINE('',#12130,#2872);
#2328=LINE('',#12132,#2873);
#2329=LINE('',#12133,#2874);
#2330=LINE('',#12136,#2875);
#2331=LINE('',#12137,#2876);
#2332=LINE('',#12140,#2877);
#2333=LINE('',#12141,#2878);
#2334=LINE('',#12142,#2879);
#2335=LINE('',#12146,#2880);
#2336=LINE('',#12148,#2881);
#2337=LINE('',#12149,#2882);
#2338=LINE('',#12152,#2883);
#2339=LINE('',#12153,#2884);
#2340=LINE('',#12157,#2885);
#2341=LINE('',#12159,#2886);
#2342=LINE('',#12161,#2887);
#2343=LINE('',#12163,#2888);
#2344=LINE('',#12165,#2889);
#2345=LINE('',#12166,#2890);
#2346=LINE('',#12170,#2891);
#2347=LINE('',#12171,#2892);
#2348=LINE('',#12174,#2893);
#2349=LINE('',#12175,#2894);
#2350=LINE('',#12177,#2895);
#2351=LINE('',#12178,#2896);
#2352=LINE('',#12180,#2897);
#2353=LINE('',#12182,#2898);
#2354=LINE('',#12187,#2899);
#2355=LINE('',#12191,#2900);
#2356=LINE('',#12199,#2901);
#2357=LINE('',#12203,#2902);
#2358=LINE('',#12207,#2903);
#2359=LINE('',#12214,#2904);
#2360=LINE('',#12221,#2905);
#2361=LINE('',#12228,#2906);
#2362=LINE('',#12234,#2907);
#2363=LINE('',#12238,#2908);
#2364=LINE('',#12242,#2909);
#2365=LINE('',#12247,#2910);
#2366=LINE('',#12251,#2911);
#2367=LINE('',#12255,#2912);
#2368=LINE('',#12260,#2913);
#2369=LINE('',#12262,#2914);
#2370=LINE('',#12283,#2915);
#2371=LINE('',#12293,#2916);
#2372=LINE('',#12300,#2917);
#2373=LINE('',#12306,#2918);
#2374=LINE('',#12312,#2919);
#2375=LINE('',#12318,#2920);
#2376=LINE('',#12323,#2921);
#2377=LINE('',#12327,#2922);
#2378=LINE('',#12329,#2923);
#2379=LINE('',#12331,#2924);
#2380=LINE('',#12332,#2925);
#2381=LINE('',#12335,#2926);
#2382=LINE('',#12337,#2927);
#2383=LINE('',#12338,#2928);
#2384=LINE('',#12341,#2929);
#2385=LINE('',#12343,#2930);
#2386=LINE('',#12344,#2931);
#2387=LINE('',#12346,#2932);
#2388=LINE('',#12347,#2933);
#2389=LINE('',#12355,#2934);
#2390=LINE('',#12360,#2935);
#2391=LINE('',#12362,#2936);
#2392=LINE('',#12364,#2937);
#2393=LINE('',#12365,#2938);
#2394=LINE('',#12376,#2939);
#2395=LINE('',#12385,#2940);
#2396=LINE('',#12388,#2941);
#2397=LINE('',#12396,#2942);
#2398=LINE('',#12398,#2943);
#2399=LINE('',#12400,#2944);
#2400=LINE('',#12402,#2945);
#2401=LINE('',#12404,#2946);
#2402=LINE('',#12405,#2947);
#2403=LINE('',#12409,#2948);
#2404=LINE('',#12411,#2949);
#2405=LINE('',#12413,#2950);
#2406=LINE('',#12414,#2951);
#2407=LINE('',#12417,#2952);
#2408=LINE('',#12418,#2953);
#2409=LINE('',#12420,#2954);
#2410=LINE('',#12421,#2955);
#2411=LINE('',#12424,#2956);
#2412=LINE('',#12425,#2957);
#2413=LINE('',#12428,#2958);
#2414=LINE('',#12429,#2959);
#2415=LINE('',#12430,#2960);
#2416=LINE('',#12434,#2961);
#2417=LINE('',#12436,#2962);
#2418=LINE('',#12437,#2963);
#2419=LINE('',#12440,#2964);
#2420=LINE('',#12441,#2965);
#2421=LINE('',#12445,#2966);
#2422=LINE('',#12447,#2967);
#2423=LINE('',#12449,#2968);
#2424=LINE('',#12451,#2969);
#2425=LINE('',#12453,#2970);
#2426=LINE('',#12454,#2971);
#2427=LINE('',#12458,#2972);
#2428=LINE('',#12459,#2973);
#2429=LINE('',#12462,#2974);
#2430=LINE('',#12463,#2975);
#2431=LINE('',#12465,#2976);
#2432=LINE('',#12466,#2977);
#2433=LINE('',#12468,#2978);
#2434=LINE('',#12470,#2979);
#2435=LINE('',#12475,#2980);
#2436=LINE('',#12479,#2981);
#2437=LINE('',#12487,#2982);
#2438=LINE('',#12491,#2983);
#2439=LINE('',#12495,#2984);
#2440=LINE('',#12502,#2985);
#2441=LINE('',#12509,#2986);
#2442=LINE('',#12515,#2987);
#2443=LINE('',#12524,#2988);
#2444=LINE('',#12530,#2989);
#2445=LINE('',#12539,#2990);
#2446=LINE('',#12545,#2991);
#2447=LINE('',#12554,#2992);
#2448=LINE('',#12563,#2993);
#2449=LINE('',#12571,#2994);
#2450=LINE('',#12575,#2995);
#2451=LINE('',#12580,#2996);
#2452=LINE('',#12589,#2997);
#2453=LINE('',#12596,#2998);
#2454=LINE('',#12600,#2999);
#2455=LINE('',#12605,#3000);
#2456=LINE('',#12607,#3001);
#2457=LINE('',#12609,#3002);
#2458=LINE('',#12610,#3003);
#2459=LINE('',#12613,#3004);
#2460=LINE('',#12615,#3005);
#2461=LINE('',#12616,#3006);
#2462=LINE('',#12619,#3007);
#2463=LINE('',#12621,#3008);
#2464=LINE('',#12622,#3009);
#2465=LINE('',#12624,#3010);
#2466=LINE('',#12625,#3011);
#2467=LINE('',#12635,#3012);
#2468=LINE('',#12639,#3013);
#2469=LINE('',#12643,#3014);
#2470=LINE('',#12650,#3015);
#2471=LINE('',#12654,#3016);
#2472=LINE('',#12658,#3017);
#2473=LINE('',#12663,#3018);
#2474=LINE('',#12665,#3019);
#2475=LINE('',#12667,#3020);
#2476=LINE('',#12668,#3021);
#2477=LINE('',#12671,#3022);
#2478=LINE('',#12673,#3023);
#2479=LINE('',#12674,#3024);
#2480=LINE('',#12677,#3025);
#2481=LINE('',#12679,#3026);
#2482=LINE('',#12680,#3027);
#2483=LINE('',#12683,#3028);
#2484=LINE('',#12685,#3029);
#2485=LINE('',#12686,#3030);
#2486=LINE('',#12689,#3031);
#2487=LINE('',#12691,#3032);
#2488=LINE('',#12692,#3033);
#2489=LINE('',#12694,#3034);
#2490=LINE('',#12695,#3035);
#2491=LINE('',#12704,#3036);
#2492=LINE('',#12712,#3037);
#2493=LINE('',#12714,#3038);
#2494=LINE('',#12716,#3039);
#2495=LINE('',#12718,#3040);
#2496=LINE('',#12720,#3041);
#2497=LINE('',#12721,#3042);
#2498=LINE('',#12727,#3043);
#2499=LINE('',#12729,#3044);
#2500=LINE('',#12731,#3045);
#2501=LINE('',#12733,#3046);
#2502=LINE('',#12735,#3047);
#2503=LINE('',#12736,#3048);
#2504=LINE('',#12740,#3049);
#2505=LINE('',#12741,#3050);
#2506=LINE('',#12743,#3051);
#2507=LINE('',#12745,#3052);
#2508=LINE('',#12747,#3053);
#2509=LINE('',#12749,#3054);
#2510=LINE('',#12756,#3055);
#2511=LINE('',#12762,#3056);
#2512=LINE('',#12766,#3057);
#2513=LINE('',#12771,#3058);
#2514=LINE('',#12781,#3059);
#2515=LINE('',#12788,#3060);
#2516=LINE('',#12793,#3061);
#2517=LINE('',#12806,#3062);
#2518=LINE('',#12816,#3063);
#2519=LINE('',#12821,#3064);
#2520=LINE('',#12826,#3065);
#2521=LINE('',#12840,#3066);
#2522=LINE('',#12849,#3067);
#2523=LINE('',#12853,#3068);
#2524=LINE('',#12860,#3069);
#2525=LINE('',#12875,#3070);
#2526=LINE('',#12896,#3071);
#2527=LINE('',#12921,#3072);
#2528=LINE('',#12922,#3073);
#2529=LINE('',#12924,#3074);
#2530=LINE('',#12926,#3075);
#2531=LINE('',#12931,#3076);
#2532=LINE('',#12934,#3077);
#2533=LINE('',#12936,#3078);
#2534=LINE('',#12945,#3079);
#2535=LINE('',#12951,#3080);
#2536=LINE('',#12957,#3081);
#2537=LINE('',#12963,#3082);
#2538=LINE('',#12969,#3083);
#2539=LINE('',#12975,#3084);
#2540=LINE('',#12981,#3085);
#2541=LINE('',#12987,#3086);
#2542=LINE('',#12993,#3087);
#2543=LINE('',#12999,#3088);
#2544=LINE('',#13005,#3089);
#2545=LINE('',#13011,#3090);
#2546=LINE('',#13017,#3091);
#2547=LINE('',#13022,#3092);
#2548=LINE('',#13024,#3093);
#2549=LINE('',#13026,#3094);
#2550=LINE('',#13027,#3095);
#2551=LINE('',#13031,#3096);
#2552=LINE('',#13033,#3097);
#2553=LINE('',#13035,#3098);
#2554=LINE('',#13036,#3099);
#2555=LINE('',#13038,#3100);
#2556=LINE('',#13039,#3101);
#2557=LINE('',#13041,#3102);
#2558=LINE('',#13043,#3103);
#2559=LINE('',#13048,#3104);
#2560=LINE('',#13054,#3105);
#2561=LINE('',#13060,#3106);
#2562=LINE('',#13066,#3107);
#2563=LINE('',#13072,#3108);
#2564=LINE('',#13077,#3109);
#2565=LINE('',#13079,#3110);
#2566=LINE('',#13081,#3111);
#2567=LINE('',#13082,#3112);
#2568=LINE('',#13086,#3113);
#2569=LINE('',#13088,#3114);
#2570=LINE('',#13090,#3115);
#2571=LINE('',#13091,#3116);
#2572=LINE('',#13093,#3117);
#2573=LINE('',#13094,#3118);
#2574=LINE('',#13096,#3119);
#2575=LINE('',#13098,#3120);
#2576=LINE('',#13102,#3121);
#2577=LINE('',#13104,#3122);
#2578=LINE('',#13106,#3123);
#2579=LINE('',#13107,#3124);
#2580=LINE('',#13110,#3125);
#2581=LINE('',#13112,#3126);
#2582=LINE('',#13113,#3127);
#2583=LINE('',#13116,#3128);
#2584=LINE('',#13118,#3129);
#2585=LINE('',#13119,#3130);
#2586=LINE('',#13121,#3131);
#2587=LINE('',#13122,#3132);
#2588=LINE('',#13130,#3133);
#2589=LINE('',#13136,#3134);
#2590=LINE('',#13142,#3135);
#2591=LINE('',#13148,#3136);
#2592=LINE('',#13154,#3137);
#2593=LINE('',#13160,#3138);
#2594=LINE('',#13169,#3139);
#2595=LINE('',#13175,#3140);
#2596=LINE('',#13181,#3141);
#2597=LINE('',#13187,#3142);
#2598=LINE('',#13193,#3143);
#2599=LINE('',#13199,#3144);
#2600=LINE('',#13208,#3145);
#2601=LINE('',#13214,#3146);
#2602=LINE('',#13220,#3147);
#2603=LINE('',#13226,#3148);
#2604=LINE('',#13232,#3149);
#2605=LINE('',#13238,#3150);
#2606=LINE('',#13247,#3151);
#2607=LINE('',#13253,#3152);
#2608=LINE('',#13259,#3153);
#2609=LINE('',#13265,#3154);
#2610=LINE('',#13271,#3155);
#2611=LINE('',#13277,#3156);
#2612=LINE('',#13288,#3157);
#2613=LINE('',#13290,#3158);
#2614=LINE('',#13291,#3159);
#2615=LINE('',#13294,#3160);
#2616=LINE('',#13296,#3161);
#2617=LINE('',#13297,#3162);
#2618=LINE('',#13302,#3163);
#2619=LINE('',#13303,#3164);
#2620=LINE('',#13305,#3165);
#2621=LINE('',#13306,#3166);
#2622=LINE('',#13316,#3167);
#2623=LINE('',#13323,#3168);
#2624=LINE('',#13330,#3169);
#2625=LINE('',#13337,#3170);
#2626=LINE('',#13344,#3171);
#2627=LINE('',#13349,#3172);
#2628=LINE('',#13356,#3173);
#2629=LINE('',#13359,#3174);
#2630=LINE('',#13362,#3175);
#2631=LINE('',#13364,#3176);
#2632=LINE('',#13365,#3177);
#2633=LINE('',#13371,#3178);
#2634=LINE('',#13373,#3179);
#2635=LINE('',#13374,#3180);
#2636=LINE('',#13383,#3181);
#2637=LINE('',#13388,#3182);
#2638=LINE('',#13395,#3183);
#2639=LINE('',#13397,#3184);
#2640=LINE('',#13399,#3185);
#2641=LINE('',#13400,#3186);
#2642=LINE('',#13403,#3187);
#2643=LINE('',#13405,#3188);
#2644=LINE('',#13406,#3189);
#2645=LINE('',#13409,#3190);
#2646=LINE('',#13411,#3191);
#2647=LINE('',#13412,#3192);
#2648=LINE('',#13415,#3193);
#2649=LINE('',#13417,#3194);
#2650=LINE('',#13418,#3195);
#2651=LINE('',#13421,#3196);
#2652=LINE('',#13423,#3197);
#2653=LINE('',#13424,#3198);
#2654=LINE('',#13426,#3199);
#2655=LINE('',#13427,#3200);
#2656=LINE('',#13439,#3201);
#2657=LINE('',#13443,#3202);
#2658=LINE('',#13447,#3203);
#2659=LINE('',#13454,#3204);
#2660=LINE('',#13456,#3205);
#2661=LINE('',#13461,#3206);
#2662=LINE('',#13463,#3207);
#2663=LINE('',#13465,#3208);
#2664=LINE('',#13466,#3209);
#2665=LINE('',#13469,#3210);
#2666=LINE('',#13471,#3211);
#2667=LINE('',#13472,#3212);
#2668=LINE('',#13475,#3213);
#2669=LINE('',#13477,#3214);
#2670=LINE('',#13478,#3215);
#2671=LINE('',#13481,#3216);
#2672=LINE('',#13483,#3217);
#2673=LINE('',#13484,#3218);
#2674=LINE('',#13487,#3219);
#2675=LINE('',#13489,#3220);
#2676=LINE('',#13490,#3221);
#2677=LINE('',#13492,#3222);
#2678=LINE('',#13493,#3223);
#2679=LINE('',#13503,#3224);
#2680=LINE('',#13512,#3225);
#2681=LINE('',#13516,#3226);
#2682=LINE('',#13520,#3227);
#2683=LINE('',#13527,#3228);
#2684=LINE('',#13531,#3229);
#2685=LINE('',#13533,#3230);
#2686=LINE('',#13608,#3231);
#2687=LINE('',#13617,#3232);
#2688=LINE('',#13627,#3233);
#2689=LINE('',#13631,#3234);
#2690=LINE('',#13636,#3235);
#2691=LINE('',#13649,#3236);
#2692=LINE('',#13656,#3237);
#2693=LINE('',#13667,#3238);
#2694=LINE('',#13671,#3239);
#2695=LINE('',#13675,#3240);
#2696=LINE('',#13682,#3241);
#2697=LINE('',#13686,#3242);
#2698=LINE('',#13690,#3243);
#2699=LINE('',#13695,#3244);
#2700=LINE('',#13697,#3245);
#2701=LINE('',#13699,#3246);
#2702=LINE('',#13700,#3247);
#2703=LINE('',#13703,#3248);
#2704=LINE('',#13705,#3249);
#2705=LINE('',#13706,#3250);
#2706=LINE('',#13709,#3251);
#2707=LINE('',#13711,#3252);
#2708=LINE('',#13712,#3253);
#2709=LINE('',#13715,#3254);
#2710=LINE('',#13717,#3255);
#2711=LINE('',#13718,#3256);
#2712=LINE('',#13721,#3257);
#2713=LINE('',#13723,#3258);
#2714=LINE('',#13724,#3259);
#2715=LINE('',#13726,#3260);
#2716=LINE('',#13727,#3261);
#2717=LINE('',#13735,#3262);
#2718=LINE('',#13741,#3263);
#2719=LINE('',#13746,#3264);
#2720=LINE('',#13763,#3265);
#2721=LINE('',#13778,#3266);
#2722=LINE('',#13783,#3267);
#2723=LINE('',#13788,#3268);
#2724=LINE('',#13790,#3269);
#2725=LINE('',#13792,#3270);
#2726=LINE('',#13793,#3271);
#2727=LINE('',#13796,#3272);
#2728=LINE('',#13798,#3273);
#2729=LINE('',#13799,#3274);
#2730=LINE('',#13802,#3275);
#2731=LINE('',#13804,#3276);
#2732=LINE('',#13805,#3277);
#2733=LINE('',#13808,#3278);
#2734=LINE('',#13810,#3279);
#2735=LINE('',#13812,#3280);
#2736=LINE('',#13814,#3281);
#2737=LINE('',#13815,#3282);
#2738=LINE('',#13818,#3283);
#2739=LINE('',#13819,#3284);
#2740=LINE('',#13822,#3285);
#2741=LINE('',#13823,#3286);
#2742=LINE('',#13826,#3287);
#2743=LINE('',#13828,#3288);
#2744=LINE('',#13829,#3289);
#2745=LINE('',#13831,#3290);
#2746=LINE('',#13833,#3291);
#2747=LINE('',#13839,#3292);
#2748=LINE('',#13841,#3293);
#2749=LINE('',#13843,#3294);
#2750=LINE('',#13844,#3295);
#2751=LINE('',#13847,#3296);
#2752=LINE('',#13849,#3297);
#2753=LINE('',#13850,#3298);
#2754=LINE('',#13853,#3299);
#2755=LINE('',#13855,#3300);
#2756=LINE('',#13856,#3301);
#2757=LINE('',#13859,#3302);
#2758=LINE('',#13861,#3303);
#2759=LINE('',#13862,#3304);
#2760=LINE('',#13865,#3305);
#2761=LINE('',#13867,#3306);
#2762=LINE('',#13868,#3307);
#2763=LINE('',#13870,#3308);
#2764=LINE('',#13871,#3309);
#2765=LINE('',#13879,#3310);
#2766=LINE('',#13883,#3311);
#2767=LINE('',#13887,#3312);
#2768=LINE('',#13904,#3313);
#2769=LINE('',#13974,#3314);
#2770=LINE('',#13978,#3315);
#2771=LINE('',#13985,#3316);
#2772=LINE('',#13986,#3317);
#2773=LINE('',#13990,#3318);
#2774=LINE('',#13997,#3319);
#2775=LINE('',#14003,#3320);
#2776=LINE('',#14070,#3321);
#2777=LINE('',#14073,#3322);
#2778=LINE('',#14075,#3323);
#2779=LINE('',#14076,#3324);
#2780=LINE('',#14080,#3325);
#2781=LINE('',#14088,#3326);
#2782=LINE('',#14095,#3327);
#2783=LINE('',#14104,#3328);
#2784=LINE('',#14111,#3329);
#2785=LINE('',#14120,#3330);
#2786=LINE('',#14126,#3331);
#2787=LINE('',#14132,#3332);
#2788=LINE('',#14137,#3333);
#2789=LINE('',#14139,#3334);
#2790=LINE('',#14141,#3335);
#2791=LINE('',#14142,#3336);
#2792=LINE('',#14145,#3337);
#2793=LINE('',#14147,#3338);
#2794=LINE('',#14148,#3339);
#2795=LINE('',#14151,#3340);
#2796=LINE('',#14152,#3341);
#2797=LINE('',#14155,#3342);
#2798=LINE('',#14156,#3343);
#2799=LINE('',#14158,#3344);
#2800=LINE('',#14162,#3345);
#2801=LINE('',#14164,#3346);
#2802=LINE('',#14166,#3347);
#2803=LINE('',#14167,#3348);
#2804=LINE('',#14170,#3349);
#2805=LINE('',#14172,#3350);
#2806=LINE('',#14173,#3351);
#2807=LINE('',#14176,#3352);
#2808=LINE('',#14178,#3353);
#2809=LINE('',#14179,#3354);
#2810=LINE('',#14181,#3355);
#2811=LINE('',#14182,#3356);
#2812=LINE('',#14190,#3357);
#2813=LINE('',#14196,#3358);
#2814=LINE('',#14212,#3359);
#2815=LINE('',#14233,#3360);
#2816=LINE('',#14258,#3361);
#2817=LINE('',#14259,#3362);
#2818=LINE('',#14261,#3363);
#2819=LINE('',#14263,#3364);
#2820=LINE('',#14268,#3365);
#2821=LINE('',#14271,#3366);
#2822=LINE('',#14273,#3367);
#2823=VECTOR('',#9391,0.21);
#2824=VECTOR('',#9400,0.21);
#2825=VECTOR('',#9407,1.);
#2826=VECTOR('',#9412,1.);
#2827=VECTOR('',#9423,1.);
#2828=VECTOR('',#9424,1.);
#2829=VECTOR('',#9429,0.2);
#2830=VECTOR('',#9432,1.);
#2831=VECTOR('',#9435,1.);
#2832=VECTOR('',#9454,1.);
#2833=VECTOR('',#9467,0.2);
#2834=VECTOR('',#9478,1.);
#2835=VECTOR('',#9489,0.685);
#2836=VECTOR('',#9498,0.275);
#2837=VECTOR('',#9505,0.275);
#2838=VECTOR('',#9512,0.275);
#2839=VECTOR('',#9519,0.275);
#2840=VECTOR('',#9526,0.6);
#2841=VECTOR('',#9533,1.);
#2842=VECTOR('',#9534,1.);
#2843=VECTOR('',#9535,1.);
#2844=VECTOR('',#9536,1.);
#2845=VECTOR('',#9539,1.);
#2846=VECTOR('',#9540,1.);
#2847=VECTOR('',#9541,1.);
#2848=VECTOR('',#9544,1.);
#2849=VECTOR('',#9545,1.);
#2850=VECTOR('',#9546,1.);
#2851=VECTOR('',#9549,1.);
#2852=VECTOR('',#9550,1.);
#2853=VECTOR('',#9561,0.515);
#2854=VECTOR('',#9566,1.);
#2855=VECTOR('',#9567,1.);
#2856=VECTOR('',#9568,1.);
#2857=VECTOR('',#9569,1.);
#2858=VECTOR('',#9584,0.49);
#2859=VECTOR('',#9597,0.25);
#2860=VECTOR('',#9600,0.25);
#2861=VECTOR('',#9609,1.);
#2862=VECTOR('',#9610,1.);
#2863=VECTOR('',#9611,1.);
#2864=VECTOR('',#9612,1.);
#2865=VECTOR('',#9613,1.);
#2866=VECTOR('',#9614,1.);
#2867=VECTOR('',#9617,1.);
#2868=VECTOR('',#9618,1.);
#2869=VECTOR('',#9619,1.);
#2870=VECTOR('',#9620,1.);
#2871=VECTOR('',#9623,1.);
#2872=VECTOR('',#9624,1.);
#2873=VECTOR('',#9625,1.);
#2874=VECTOR('',#9626,1.);
#2875=VECTOR('',#9629,1.);
#2876=VECTOR('',#9630,1.);
#2877=VECTOR('',#9633,1.);
#2878=VECTOR('',#9634,1.);
#2879=VECTOR('',#9635,1.);
#2880=VECTOR('',#9640,1.);
#2881=VECTOR('',#9641,1.);
#2882=VECTOR('',#9642,1.);
#2883=VECTOR('',#9645,1.);
#2884=VECTOR('',#9646,1.);
#2885=VECTOR('',#9649,1.);
#2886=VECTOR('',#9650,1.);
#2887=VECTOR('',#9651,1.);
#2888=VECTOR('',#9652,1.);
#2889=VECTOR('',#9653,1.);
#2890=VECTOR('',#9654,1.);
#2891=VECTOR('',#9659,1.);
#2892=VECTOR('',#9660,1.);
#2893=VECTOR('',#9663,1.);
#2894=VECTOR('',#9664,1.);
#2895=VECTOR('',#9667,1.);
#2896=VECTOR('',#9668,1.);
#2897=VECTOR('',#9671,1.);
#2898=VECTOR('',#9674,1.);
#2899=VECTOR('',#9681,0.2);
#2900=VECTOR('',#9686,0.685);
#2901=VECTOR('',#9697,0.1);
#2902=VECTOR('',#9702,0.25);
#2903=VECTOR('',#9707,0.3);
#2904=VECTOR('',#9716,0.6);
#2905=VECTOR('',#9725,0.21);
#2906=VECTOR('',#9734,0.21);
#2907=VECTOR('',#9741,1.);
#2908=VECTOR('',#9746,1.);
#2909=VECTOR('',#9751,1.);
#2910=VECTOR('',#9756,1.);
#2911=VECTOR('',#9759,1.);
#2912=VECTOR('',#9762,0.2);
#2913=VECTOR('',#9767,1.);
#2914=VECTOR('',#9768,1.);
#2915=VECTOR('',#9807,0.2);
#2916=VECTOR('',#9820,0.685);
#2917=VECTOR('',#9829,0.275);
#2918=VECTOR('',#9836,0.275);
#2919=VECTOR('',#9843,0.275);
#2920=VECTOR('',#9850,0.275);
#2921=VECTOR('',#9857,1.);
#2922=VECTOR('',#9860,1.);
#2923=VECTOR('',#9861,1.);
#2924=VECTOR('',#9862,1.);
#2925=VECTOR('',#9863,1.);
#2926=VECTOR('',#9866,1.);
#2927=VECTOR('',#9867,1.);
#2928=VECTOR('',#9868,1.);
#2929=VECTOR('',#9871,1.);
#2930=VECTOR('',#9872,1.);
#2931=VECTOR('',#9873,1.);
#2932=VECTOR('',#9876,1.);
#2933=VECTOR('',#9877,1.);
#2934=VECTOR('',#9888,0.515);
#2935=VECTOR('',#9893,1.);
#2936=VECTOR('',#9894,1.);
#2937=VECTOR('',#9895,1.);
#2938=VECTOR('',#9896,1.);
#2939=VECTOR('',#9911,0.49);
#2940=VECTOR('',#9924,0.25);
#2941=VECTOR('',#9927,0.25);
#2942=VECTOR('',#9936,1.);
#2943=VECTOR('',#9937,1.);
#2944=VECTOR('',#9938,1.);
#2945=VECTOR('',#9939,1.);
#2946=VECTOR('',#9940,1.);
#2947=VECTOR('',#9941,1.);
#2948=VECTOR('',#9944,1.);
#2949=VECTOR('',#9945,1.);
#2950=VECTOR('',#9946,1.);
#2951=VECTOR('',#9947,1.);
#2952=VECTOR('',#9950,1.);
#2953=VECTOR('',#9951,1.);
#2954=VECTOR('',#9952,1.);
#2955=VECTOR('',#9953,1.);
#2956=VECTOR('',#9956,1.);
#2957=VECTOR('',#9957,1.);
#2958=VECTOR('',#9960,1.);
#2959=VECTOR('',#9961,1.);
#2960=VECTOR('',#9962,1.);
#2961=VECTOR('',#9967,1.);
#2962=VECTOR('',#9968,1.);
#2963=VECTOR('',#9969,1.);
#2964=VECTOR('',#9972,1.);
#2965=VECTOR('',#9973,1.);
#2966=VECTOR('',#9976,1.);
#2967=VECTOR('',#9977,1.);
#2968=VECTOR('',#9978,1.);
#2969=VECTOR('',#9979,1.);
#2970=VECTOR('',#9980,1.);
#2971=VECTOR('',#9981,1.);
#2972=VECTOR('',#9986,1.);
#2973=VECTOR('',#9987,1.);
#2974=VECTOR('',#9990,1.);
#2975=VECTOR('',#9991,1.);
#2976=VECTOR('',#9994,1.);
#2977=VECTOR('',#9995,1.);
#2978=VECTOR('',#9998,1.);
#2979=VECTOR('',#10001,1.);
#2980=VECTOR('',#10008,0.2);
#2981=VECTOR('',#10013,0.685);
#2982=VECTOR('',#10024,0.1);
#2983=VECTOR('',#10029,0.25);
#2984=VECTOR('',#10034,0.3);
#2985=VECTOR('',#10043,0.6);
#2986=VECTOR('',#10052,1.);
#2987=VECTOR('',#10059,1.6);
#2988=VECTOR('',#10072,1.);
#2989=VECTOR('',#10079,1.6);
#2990=VECTOR('',#10092,1.);
#2991=VECTOR('',#10099,1.6);
#2992=VECTOR('',#10112,0.45);
#2993=VECTOR('',#10123,0.45);
#2994=VECTOR('',#10134,0.275);
#2995=VECTOR('',#10139,0.275);
#2996=VECTOR('',#10144,0.5);
#2997=VECTOR('',#10155,0.5);
#2998=VECTOR('',#10164,0.275);
#2999=VECTOR('',#10169,0.275);
#3000=VECTOR('',#10174,1.);
#3001=VECTOR('',#10175,1.);
#3002=VECTOR('',#10176,1.);
#3003=VECTOR('',#10177,1.);
#3004=VECTOR('',#10180,1.);
#3005=VECTOR('',#10181,1.);
#3006=VECTOR('',#10182,1.);
#3007=VECTOR('',#10185,1.);
#3008=VECTOR('',#10186,1.);
#3009=VECTOR('',#10187,1.);
#3010=VECTOR('',#10190,1.);
#3011=VECTOR('',#10191,1.);
#3012=VECTOR('',#10206,0.4);
#3013=VECTOR('',#10211,0.425);
#3014=VECTOR('',#10216,0.41);
#3015=VECTOR('',#10225,0.26);
#3016=VECTOR('',#10230,0.25);
#3017=VECTOR('',#10235,0.225);
#3018=VECTOR('',#10240,1.);
#3019=VECTOR('',#10241,1.);
#3020=VECTOR('',#10242,1.);
#3021=VECTOR('',#10243,1.);
#3022=VECTOR('',#10246,1.);
#3023=VECTOR('',#10247,1.);
#3024=VECTOR('',#10248,1.);
#3025=VECTOR('',#10251,1.);
#3026=VECTOR('',#10252,1.);
#3027=VECTOR('',#10253,1.);
#3028=VECTOR('',#10256,1.);
#3029=VECTOR('',#10257,1.);
#3030=VECTOR('',#10258,1.);
#3031=VECTOR('',#10261,1.);
#3032=VECTOR('',#10262,1.);
#3033=VECTOR('',#10263,1.);
#3034=VECTOR('',#10266,1.);
#3035=VECTOR('',#10267,1.);
#3036=VECTOR('',#10280,0.43);
#3037=VECTOR('',#10289,1.);
#3038=VECTOR('',#10290,1.);
#3039=VECTOR('',#10291,1.);
#3040=VECTOR('',#10292,1.);
#3041=VECTOR('',#10293,1.);
#3042=VECTOR('',#10294,1.);
#3043=VECTOR('',#10299,1.);
#3044=VECTOR('',#10300,1.);
#3045=VECTOR('',#10301,1.);
#3046=VECTOR('',#10302,1.);
#3047=VECTOR('',#10303,1.);
#3048=VECTOR('',#10304,1.);
#3049=VECTOR('',#10309,1.);
#3050=VECTOR('',#10310,1.);
#3051=VECTOR('',#10313,1.);
#3052=VECTOR('',#10316,1.);
#3053=VECTOR('',#10319,1.);
#3054=VECTOR('',#10322,1.);
#3055=VECTOR('',#10331,0.46);
#3056=VECTOR('',#10340,0.525);
#3057=VECTOR('',#10345,0.515);
#3058=VECTOR('',#10352,0.2);
#3059=VECTOR('',#10365,0.475);
#3060=VECTOR('',#10374,0.355);
#3061=VECTOR('',#10381,0.31);
#3062=VECTOR('',#10400,0.51);
#3063=VECTOR('',#10413,0.405);
#3064=VECTOR('',#10420,0.405);
#3065=VECTOR('',#10425,0.6);
#3066=VECTOR('',#10446,0.25);
#3067=VECTOR('',#10459,0.275);
#3068=VECTOR('',#10464,0.265);
#3069=VECTOR('',#10473,0.5);
#3070=VECTOR('',#10482,0.47094010767585);
#3071=VECTOR('',#10489,0.47094010767585);
#3072=VECTOR('',#10492,1.);
#3073=VECTOR('',#10493,1.);
#3074=VECTOR('',#10496,1.);
#3075=VECTOR('',#10499,1.);
#3076=VECTOR('',#10504,0.25);
#3077=VECTOR('',#10509,1.);
#3078=VECTOR('',#10512,1.);
#3079=VECTOR('',#10525,0.33);
#3080=VECTOR('',#10532,0.33);
#3081=VECTOR('',#10539,0.33);
#3082=VECTOR('',#10546,0.33);
#3083=VECTOR('',#10553,0.21);
#3084=VECTOR('',#10560,0.21);
#3085=VECTOR('',#10567,0.21);
#3086=VECTOR('',#10574,0.21);
#3087=VECTOR('',#10581,0.165);
#3088=VECTOR('',#10588,0.165);
#3089=VECTOR('',#10595,0.165);
#3090=VECTOR('',#10602,0.165);
#3091=VECTOR('',#10609,1.05);
#3092=VECTOR('',#10614,1.);
#3093=VECTOR('',#10615,1.);
#3094=VECTOR('',#10616,1.);
#3095=VECTOR('',#10617,1.);
#3096=VECTOR('',#10620,1.);
#3097=VECTOR('',#10621,1.);
#3098=VECTOR('',#10622,1.);
#3099=VECTOR('',#10623,1.);
#3100=VECTOR('',#10626,1.);
#3101=VECTOR('',#10627,1.);
#3102=VECTOR('',#10630,1.);
#3103=VECTOR('',#10633,1.);
#3104=VECTOR('',#10638,0.165);
#3105=VECTOR('',#10645,0.165);
#3106=VECTOR('',#10652,0.165);
#3107=VECTOR('',#10659,0.165);
#3108=VECTOR('',#10666,1.05);
#3109=VECTOR('',#10671,1.);
#3110=VECTOR('',#10672,1.);
#3111=VECTOR('',#10673,1.);
#3112=VECTOR('',#10674,1.);
#3113=VECTOR('',#10677,1.);
#3114=VECTOR('',#10678,1.);
#3115=VECTOR('',#10679,1.);
#3116=VECTOR('',#10680,1.);
#3117=VECTOR('',#10683,1.);
#3118=VECTOR('',#10684,1.);
#3119=VECTOR('',#10687,1.);
#3120=VECTOR('',#10690,1.);
#3121=VECTOR('',#10693,1.);
#3122=VECTOR('',#10694,1.);
#3123=VECTOR('',#10695,1.);
#3124=VECTOR('',#10696,1.);
#3125=VECTOR('',#10699,1.);
#3126=VECTOR('',#10700,1.);
#3127=VECTOR('',#10701,1.);
#3128=VECTOR('',#10704,1.);
#3129=VECTOR('',#10705,1.);
#3130=VECTOR('',#10706,1.);
#3131=VECTOR('',#10709,1.);
#3132=VECTOR('',#10710,1.);
#3133=VECTOR('',#10721,0.225);
#3134=VECTOR('',#10728,0.225);
#3135=VECTOR('',#10735,0.225);
#3136=VECTOR('',#10742,0.225);
#3137=VECTOR('',#10749,0.62);
#3138=VECTOR('',#10756,2.);
#3139=VECTOR('',#10769,0.225);
#3140=VECTOR('',#10776,0.225);
#3141=VECTOR('',#10783,0.225);
#3142=VECTOR('',#10790,0.225);
#3143=VECTOR('',#10797,0.62);
#3144=VECTOR('',#10804,2.);
#3145=VECTOR('',#10817,0.225);
#3146=VECTOR('',#10824,0.225);
#3147=VECTOR('',#10831,0.225);
#3148=VECTOR('',#10838,0.225);
#3149=VECTOR('',#10845,0.62);
#3150=VECTOR('',#10852,2.);
#3151=VECTOR('',#10865,0.225);
#3152=VECTOR('',#10872,0.225);
#3153=VECTOR('',#10879,0.225);
#3154=VECTOR('',#10886,0.225);
#3155=VECTOR('',#10893,0.62);
#3156=VECTOR('',#10900,2.);
#3157=VECTOR('',#10915,1.);
#3158=VECTOR('',#10916,1.);
#3159=VECTOR('',#10917,1.);
#3160=VECTOR('',#10920,1.);
#3161=VECTOR('',#10921,1.);
#3162=VECTOR('',#10922,1.);
#3163=VECTOR('',#10927,1.);
#3164=VECTOR('',#10928,1.);
#3165=VECTOR('',#10931,1.);
#3166=VECTOR('',#10932,1.);
#3167=VECTOR('',#10945,1.05);
#3168=VECTOR('',#10954,1.);
#3169=VECTOR('',#10963,1.05);
#3170=VECTOR('',#10972,1.);
#3171=VECTOR('',#10981,1.05);
#3172=VECTOR('',#10988,0.9);
#3173=VECTOR('',#10995,1.);
#3174=VECTOR('',#10998,1.);
#3175=VECTOR('',#11001,1.);
#3176=VECTOR('',#11002,1.);
#3177=VECTOR('',#11003,1.);
#3178=VECTOR('',#11010,1.);
#3179=VECTOR('',#11013,1.);
#3180=VECTOR('',#11014,1.);
#3181=VECTOR('',#11025,0.895);
#3182=VECTOR('',#11032,0.605);
#3183=VECTOR('',#11041,1.);
#3184=VECTOR('',#11042,1.);
#3185=VECTOR('',#11043,1.);
#3186=VECTOR('',#11044,1.);
#3187=VECTOR('',#11047,1.);
#3188=VECTOR('',#11048,1.);
#3189=VECTOR('',#11049,1.);
#3190=VECTOR('',#11052,1.);
#3191=VECTOR('',#11053,1.);
#3192=VECTOR('',#11054,1.);
#3193=VECTOR('',#11057,1.);
#3194=VECTOR('',#11058,1.);
#3195=VECTOR('',#11059,1.);
#3196=VECTOR('',#11062,1.);
#3197=VECTOR('',#11063,1.);
#3198=VECTOR('',#11064,1.);
#3199=VECTOR('',#11067,1.);
#3200=VECTOR('',#11068,1.);
#3201=VECTOR('',#11085,0.325);
#3202=VECTOR('',#11090,0.35);
#3203=VECTOR('',#11095,0.335);
#3204=VECTOR('',#11104,0.21);
#3205=VECTOR('',#11107,0.2);
#3206=VECTOR('',#11112,1.);
#3207=VECTOR('',#11113,1.);
#3208=VECTOR('',#11114,1.);
#3209=VECTOR('',#11115,1.);
#3210=VECTOR('',#11118,1.);
#3211=VECTOR('',#11119,1.);
#3212=VECTOR('',#11120,1.);
#3213=VECTOR('',#11123,1.);
#3214=VECTOR('',#11124,1.);
#3215=VECTOR('',#11125,1.);
#3216=VECTOR('',#11128,1.);
#3217=VECTOR('',#11129,1.);
#3218=VECTOR('',#11130,1.);
#3219=VECTOR('',#11133,1.);
#3220=VECTOR('',#11134,1.);
#3221=VECTOR('',#11135,1.);
#3222=VECTOR('',#11138,1.);
#3223=VECTOR('',#11139,1.);
#3224=VECTOR('',#11152,0.25);
#3225=VECTOR('',#11165,0.4);
#3226=VECTOR('',#11170,0.425);
#3227=VECTOR('',#11175,0.41);
#3228=VECTOR('',#11184,0.26);
#3229=VECTOR('',#11189,0.25);
#3230=VECTOR('',#11192,0.225);
#3231=VECTOR('',#11337,0.4);
#3232=VECTOR('',#11348,0.9);
#3233=VECTOR('',#11361,0.99);
#3234=VECTOR('',#11366,0.225);
#3235=VECTOR('',#11373,0.99);
#3236=VECTOR('',#11392,0.165);
#3237=VECTOR('',#11401,0.4);
#3238=VECTOR('',#11418,0.325);
#3239=VECTOR('',#11423,0.35);
#3240=VECTOR('',#11428,0.335);
#3241=VECTOR('',#11437,0.21);
#3242=VECTOR('',#11442,0.2);
#3243=VECTOR('',#11447,0.18);
#3244=VECTOR('',#11452,1.);
#3245=VECTOR('',#11453,1.);
#3246=VECTOR('',#11454,1.);
#3247=VECTOR('',#11455,1.);
#3248=VECTOR('',#11458,1.);
#3249=VECTOR('',#11459,1.);
#3250=VECTOR('',#11460,1.);
#3251=VECTOR('',#11463,1.);
#3252=VECTOR('',#11464,1.);
#3253=VECTOR('',#11465,1.);
#3254=VECTOR('',#11468,1.);
#3255=VECTOR('',#11469,1.);
#3256=VECTOR('',#11470,1.);
#3257=VECTOR('',#11473,1.);
#3258=VECTOR('',#11474,1.);
#3259=VECTOR('',#11475,1.);
#3260=VECTOR('',#11478,1.);
#3261=VECTOR('',#11479,1.);
#3262=VECTOR('',#11490,0.305);
#3263=VECTOR('',#11497,0.305);
#3264=VECTOR('',#11502,1.);
#3265=VECTOR('',#11509,0.165);
#3266=VECTOR('',#11516,1.);
#3267=VECTOR('',#11521,0.4);
#3268=VECTOR('',#11526,1.);
#3269=VECTOR('',#11527,1.);
#3270=VECTOR('',#11528,1.);
#3271=VECTOR('',#11529,1.);
#3272=VECTOR('',#11532,1.);
#3273=VECTOR('',#11533,1.);
#3274=VECTOR('',#11534,1.);
#3275=VECTOR('',#11537,1.);
#3276=VECTOR('',#11538,1.);
#3277=VECTOR('',#11539,1.);
#3278=VECTOR('',#11542,1.);
#3279=VECTOR('',#11543,1.);
#3280=VECTOR('',#11544,1.);
#3281=VECTOR('',#11545,1.);
#3282=VECTOR('',#11546,1.);
#3283=VECTOR('',#11549,1.);
#3284=VECTOR('',#11550,1.);
#3285=VECTOR('',#11553,1.);
#3286=VECTOR('',#11554,1.);
#3287=VECTOR('',#11557,1.);
#3288=VECTOR('',#11558,1.);
#3289=VECTOR('',#11559,1.);
#3290=VECTOR('',#11562,1.);
#3291=VECTOR('',#11565,1.);
#3292=VECTOR('',#11572,1.);
#3293=VECTOR('',#11573,1.);
#3294=VECTOR('',#11574,1.);
#3295=VECTOR('',#11575,1.);
#3296=VECTOR('',#11578,1.);
#3297=VECTOR('',#11579,1.);
#3298=VECTOR('',#11580,1.);
#3299=VECTOR('',#11583,1.);
#3300=VECTOR('',#11584,1.);
#3301=VECTOR('',#11585,1.);
#3302=VECTOR('',#11588,1.);
#3303=VECTOR('',#11589,1.);
#3304=VECTOR('',#11590,1.);
#3305=VECTOR('',#11593,1.);
#3306=VECTOR('',#11594,1.);
#3307=VECTOR('',#11595,1.);
#3308=VECTOR('',#11598,1.);
#3309=VECTOR('',#11599,1.);
#3310=VECTOR('',#11610,0.185);
#3311=VECTOR('',#11615,0.2);
#3312=VECTOR('',#11620,0.1625);
#3313=VECTOR('',#11627,0.08);
#3314=VECTOR('',#11636,0.475);
#3315=VECTOR('',#11641,0.5);
#3316=VECTOR('',#11650,0.3);
#3317=VECTOR('',#11651,0.3);
#3318=VECTOR('',#11656,0.255);
#3319=VECTOR('',#11665,0.32);
#3320=VECTOR('',#11672,0.6);
#3321=VECTOR('',#11691,1.);
#3322=VECTOR('',#11694,1.);
#3323=VECTOR('',#11695,1.);
#3324=VECTOR('',#11696,1.);
#3325=VECTOR('',#11701,0.08);
#3326=VECTOR('',#11712,0.3);
#3327=VECTOR('',#11721,0.6);
#3328=VECTOR('',#11734,0.3);
#3329=VECTOR('',#11743,0.6);
#3330=VECTOR('',#11756,0.325);
#3331=VECTOR('',#11763,0.325);
#3332=VECTOR('',#11770,0.31);
#3333=VECTOR('',#11775,1.);
#3334=VECTOR('',#11776,1.);
#3335=VECTOR('',#11777,1.);
#3336=VECTOR('',#11778,1.);
#3337=VECTOR('',#11781,1.);
#3338=VECTOR('',#11782,1.);
#3339=VECTOR('',#11783,1.);
#3340=VECTOR('',#11786,1.);
#3341=VECTOR('',#11787,1.);
#3342=VECTOR('',#11790,1.);
#3343=VECTOR('',#11791,1.);
#3344=VECTOR('',#11794,1.);
#3345=VECTOR('',#11797,1.);
#3346=VECTOR('',#11798,1.);
#3347=VECTOR('',#11799,1.);
#3348=VECTOR('',#11800,1.);
#3349=VECTOR('',#11803,1.);
#3350=VECTOR('',#11804,1.);
#3351=VECTOR('',#11805,1.);
#3352=VECTOR('',#11808,1.);
#3353=VECTOR('',#11809,1.);
#3354=VECTOR('',#11810,1.);
#3355=VECTOR('',#11813,1.);
#3356=VECTOR('',#11814,1.);
#3357=VECTOR('',#11825,0.32);
#3358=VECTOR('',#11832,0.6);
#3359=VECTOR('',#11843,0.576175134594813);
#3360=VECTOR('',#11850,0.576175134594813);
#3361=VECTOR('',#11853,1.);
#3362=VECTOR('',#11854,1.);
#3363=VECTOR('',#11857,1.);
#3364=VECTOR('',#11860,1.);
#3365=VECTOR('',#11865,0.3);
#3366=VECTOR('',#11870,1.);
#3367=VECTOR('',#11873,1.);
#3368=CIRCLE('',#8388,0.21);
#3369=CIRCLE('',#8389,0.21);
#3370=CIRCLE('',#8392,0.21);
#3371=CIRCLE('',#8393,0.21);
#3372=CIRCLE('',#8396,0.2);
#3373=CIRCLE('',#8398,0.2);
#3374=CIRCLE('',#8405,0.2);
#3375=CIRCLE('',#8406,0.2);
#3376=CIRCLE('',#8407,0.2);
#3377=CIRCLE('',#8411,0.2);
#3378=CIRCLE('',#8414,1.);
#3379=CIRCLE('',#8417,0.2);
#3380=CIRCLE('',#8419,0.2);
#3381=CIRCLE('',#8422,0.2);
#3382=CIRCLE('',#8424,0.2);
#3383=CIRCLE('',#8426,1.);
#3384=CIRCLE('',#8427,1.);
#3385=CIRCLE('',#8428,1.);
#3386=CIRCLE('',#8431,0.685);
#3387=CIRCLE('',#8432,0.685);
#3388=CIRCLE('',#8435,0.275);
#3389=CIRCLE('',#8436,0.275);
#3390=CIRCLE('',#8438,0.275);
#3391=CIRCLE('',#8439,0.275);
#3392=CIRCLE('',#8441,0.275);
#3393=CIRCLE('',#8442,0.275);
#3394=CIRCLE('',#8444,0.275);
#3395=CIRCLE('',#8445,0.275);
#3396=CIRCLE('',#8447,0.6);
#3397=CIRCLE('',#8448,0.6);
#3398=CIRCLE('',#8458,0.515);
#3399=CIRCLE('',#8459,0.515);
#3400=CIRCLE('',#8462,0.4);
#3401=CIRCLE('',#8463,0.25);
#3402=CIRCLE('',#8465,0.4);
#3403=CIRCLE('',#8467,0.49);
#3404=CIRCLE('',#8468,0.49);
#3405=CIRCLE('',#8470,0.25);
#3406=CIRCLE('',#8472,0.25);
#3407=CIRCLE('',#8475,0.25);
#3408=CIRCLE('',#8477,0.2);
#3409=CIRCLE('',#8487,0.685);
#3410=CIRCLE('',#8496,0.2);
#3411=CIRCLE('',#8498,0.685);
#3412=CIRCLE('',#8502,0.2);
#3413=CIRCLE('',#8504,0.3);
#3414=CIRCLE('',#8506,0.3);
#3415=CIRCLE('',#8508,0.6);
#3416=CIRCLE('',#8510,0.6);
#3417=CIRCLE('',#8514,0.21);
#3418=CIRCLE('',#8515,0.21);
#3419=CIRCLE('',#8518,0.21);
#3420=CIRCLE('',#8519,0.21);
#3421=CIRCLE('',#8522,0.2);
#3422=CIRCLE('',#8524,0.2);
#3423=CIRCLE('',#8526,0.2);
#3424=CIRCLE('',#8528,0.2);
#3425=CIRCLE('',#8529,0.2);
#3426=CIRCLE('',#8533,0.2);
#3427=CIRCLE('',#8541,1.);
#3428=CIRCLE('',#8543,0.2);
#3429=CIRCLE('',#8545,0.2);
#3430=CIRCLE('',#8547,0.2);
#3431=CIRCLE('',#8551,0.2);
#3432=CIRCLE('',#8553,1.);
#3433=CIRCLE('',#8554,1.);
#3434=CIRCLE('',#8556,0.685);
#3435=CIRCLE('',#8557,0.685);
#3436=CIRCLE('',#8560,0.275);
#3437=CIRCLE('',#8561,0.275);
#3438=CIRCLE('',#8563,0.275);
#3439=CIRCLE('',#8564,0.275);
#3440=CIRCLE('',#8566,0.275);
#3441=CIRCLE('',#8567,0.275);
#3442=CIRCLE('',#8569,0.275);
#3443=CIRCLE('',#8570,0.275);
#3444=CIRCLE('',#8572,1.);
#3445=CIRCLE('',#8581,0.515);
#3446=CIRCLE('',#8582,0.515);
#3447=CIRCLE('',#8585,0.4);
#3448=CIRCLE('',#8586,0.25);
#3449=CIRCLE('',#8588,0.4);
#3450=CIRCLE('',#8590,0.49);
#3451=CIRCLE('',#8591,0.49);
#3452=CIRCLE('',#8593,0.25);
#3453=CIRCLE('',#8595,0.25);
#3454=CIRCLE('',#8598,0.25);
#3455=CIRCLE('',#8600,0.2);
#3456=CIRCLE('',#8610,0.685);
#3457=CIRCLE('',#8619,0.2);
#3458=CIRCLE('',#8621,0.685);
#3459=CIRCLE('',#8625,0.2);
#3460=CIRCLE('',#8627,0.3);
#3461=CIRCLE('',#8629,0.3);
#3462=CIRCLE('',#8631,0.6);
#3463=CIRCLE('',#8633,0.6);
#3464=CIRCLE('',#8637,1.);
#3465=CIRCLE('',#8638,1.);
#3466=CIRCLE('',#8640,1.6);
#3467=CIRCLE('',#8641,1.6);
#3468=CIRCLE('',#8646,1.);
#3469=CIRCLE('',#8647,1.);
#3470=CIRCLE('',#8649,1.6);
#3471=CIRCLE('',#8650,1.6);
#3472=CIRCLE('',#8655,1.);
#3473=CIRCLE('',#8656,1.);
#3474=CIRCLE('',#8658,1.6);
#3475=CIRCLE('',#8659,1.6);
#3476=CIRCLE('',#8664,0.45);
#3477=CIRCLE('',#8665,0.45);
#3478=CIRCLE('',#8667,0.275);
#3479=CIRCLE('',#8669,0.45);
#3480=CIRCLE('',#8670,0.45);
#3481=CIRCLE('',#8672,0.275);
#3482=CIRCLE('',#8674,0.275);
#3483=CIRCLE('',#8676,0.275);
#3484=CIRCLE('',#8678,0.5);
#3485=CIRCLE('',#8679,0.5);
#3486=CIRCLE('',#8681,0.275);
#3487=CIRCLE('',#8683,0.5);
#3488=CIRCLE('',#8684,0.5);
#3489=CIRCLE('',#8686,0.275);
#3490=CIRCLE('',#8688,0.275);
#3491=CIRCLE('',#8690,0.275);
#3492=CIRCLE('',#8699,0.375);
#3493=CIRCLE('',#8701,0.425);
#3494=CIRCLE('',#8703,0.425);
#3495=CIRCLE('',#8705,0.395);
#3496=CIRCLE('',#8707,0.27);
#3497=CIRCLE('',#8709,0.24505);
#3498=CIRCLE('',#8711,0.24505);
#3499=CIRCLE('',#8713,0.2);
#3500=CIRCLE('',#8726,0.43);
#3501=CIRCLE('',#8727,0.43);
#3502=CIRCLE('',#8729,0.2);
#3503=CIRCLE('',#8731,0.525);
#3504=CIRCLE('',#8733,0.515);
#3505=CIRCLE('',#8741,0.46);
#3506=CIRCLE('',#8743,0.46);
#3507=CIRCLE('',#8745,0.525);
#3508=CIRCLE('',#8748,0.515);
#3509=CIRCLE('',#8750,0.2);
#3510=CIRCLE('',#8754,0.475);
#3511=CIRCLE('',#8755,0.31);
#3512=CIRCLE('',#8757,0.475);
#3513=CIRCLE('',#8759,0.355);
#3514=CIRCLE('',#8761,0.355);
#3515=CIRCLE('',#8763,0.31);
#3516=CIRCLE('',#8769,0.089);
#3517=CIRCLE('',#8770,0.3035);
#3518=CIRCLE('',#8773,0.51);
#3519=CIRCLE('',#8774,0.51);
#3520=CIRCLE('',#8776,0.405);
#3521=CIRCLE('',#8778,0.405);
#3522=CIRCLE('',#8780,0.405);
#3523=CIRCLE('',#8782,0.405);
#3524=CIRCLE('',#8784,0.6);
#3525=CIRCLE('',#8785,0.6);
#3526=CIRCLE('',#8790,0.05);
#3527=CIRCLE('',#8791,0.4);
#3528=CIRCLE('',#8794,0.25);
#3529=CIRCLE('',#8795,0.25);
#3530=CIRCLE('',#8800,0.285);
#3531=CIRCLE('',#8801,0.265);
#3532=CIRCLE('',#8803,0.265);
#3533=CIRCLE('',#8805,0.5);
#3534=CIRCLE('',#8807,0.5);
#3535=CIRCLE('',#8811,0.38);
#3536=CIRCLE('',#8813,0.38);
#3537=CIRCLE('',#8818,0.2117);
#3538=CIRCLE('',#8819,0.2117);
#3539=CIRCLE('',#8827,0.33);
#3540=CIRCLE('',#8828,0.33);
#3541=CIRCLE('',#8830,0.33);
#3542=CIRCLE('',#8831,0.33);
#3543=CIRCLE('',#8833,0.33);
#3544=CIRCLE('',#8834,0.33);
#3545=CIRCLE('',#8836,0.33);
#3546=CIRCLE('',#8837,0.33);
#3547=CIRCLE('',#8839,0.21);
#3548=CIRCLE('',#8840,0.21);
#3549=CIRCLE('',#8842,0.21);
#3550=CIRCLE('',#8843,0.21);
#3551=CIRCLE('',#8845,0.21);
#3552=CIRCLE('',#8846,0.21);
#3553=CIRCLE('',#8848,0.21);
#3554=CIRCLE('',#8849,0.21);
#3555=CIRCLE('',#8851,0.165);
#3556=CIRCLE('',#8852,0.165);
#3557=CIRCLE('',#8854,0.165);
#3558=CIRCLE('',#8855,0.165);
#3559=CIRCLE('',#8857,0.165);
#3560=CIRCLE('',#8858,0.165);
#3561=CIRCLE('',#8860,0.165);
#3562=CIRCLE('',#8861,0.165);
#3563=CIRCLE('',#8863,1.05);
#3564=CIRCLE('',#8864,1.05);
#3565=CIRCLE('',#8871,0.165);
#3566=CIRCLE('',#8872,0.165);
#3567=CIRCLE('',#8874,0.165);
#3568=CIRCLE('',#8875,0.165);
#3569=CIRCLE('',#8877,0.165);
#3570=CIRCLE('',#8878,0.165);
#3571=CIRCLE('',#8880,0.165);
#3572=CIRCLE('',#8881,0.165);
#3573=CIRCLE('',#8883,1.05);
#3574=CIRCLE('',#8884,1.05);
#3575=CIRCLE('',#8898,0.225);
#3576=CIRCLE('',#8899,0.225);
#3577=CIRCLE('',#8901,0.225);
#3578=CIRCLE('',#8902,0.225);
#3579=CIRCLE('',#8904,0.225);
#3580=CIRCLE('',#8905,0.225);
#3581=CIRCLE('',#8907,0.225);
#3582=CIRCLE('',#8908,0.225);
#3583=CIRCLE('',#8910,0.62);
#3584=CIRCLE('',#8911,0.62);
#3585=CIRCLE('',#8913,2.);
#3586=CIRCLE('',#8914,2.);
#3587=CIRCLE('',#8919,0.225);
#3588=CIRCLE('',#8920,0.225);
#3589=CIRCLE('',#8922,0.225);
#3590=CIRCLE('',#8923,0.225);
#3591=CIRCLE('',#8925,0.225);
#3592=CIRCLE('',#8926,0.225);
#3593=CIRCLE('',#8928,0.225);
#3594=CIRCLE('',#8929,0.225);
#3595=CIRCLE('',#8931,0.62);
#3596=CIRCLE('',#8932,0.62);
#3597=CIRCLE('',#8934,2.);
#3598=CIRCLE('',#8935,2.);
#3599=CIRCLE('',#8940,0.225);
#3600=CIRCLE('',#8941,0.225);
#3601=CIRCLE('',#8943,0.225);
#3602=CIRCLE('',#8944,0.225);
#3603=CIRCLE('',#8946,0.225);
#3604=CIRCLE('',#8947,0.225);
#3605=CIRCLE('',#8949,0.225);
#3606=CIRCLE('',#8950,0.225);
#3607=CIRCLE('',#8952,0.62);
#3608=CIRCLE('',#8953,0.62);
#3609=CIRCLE('',#8955,2.);
#3610=CIRCLE('',#8956,2.);
#3611=CIRCLE('',#8961,0.225);
#3612=CIRCLE('',#8962,0.225);
#3613=CIRCLE('',#8964,0.225);
#3614=CIRCLE('',#8965,0.225);
#3615=CIRCLE('',#8967,0.225);
#3616=CIRCLE('',#8968,0.225);
#3617=CIRCLE('',#8970,0.225);
#3618=CIRCLE('',#8971,0.225);
#3619=CIRCLE('',#8973,0.62);
#3620=CIRCLE('',#8974,0.62);
#3621=CIRCLE('',#8976,2.);
#3622=CIRCLE('',#8977,2.);
#3623=CIRCLE('',#8983,0.9);
#3624=CIRCLE('',#8986,0.9);
#3625=CIRCLE('',#8990,1.05);
#3626=CIRCLE('',#8991,0.9);
#3627=CIRCLE('',#8993,1.05);
#3628=CIRCLE('',#8995,1.);
#3629=CIRCLE('',#8997,1.);
#3630=CIRCLE('',#8999,1.05);
#3631=CIRCLE('',#9001,1.05);
#3632=CIRCLE('',#9003,1.);
#3633=CIRCLE('',#9005,1.);
#3634=CIRCLE('',#9007,1.05);
#3635=CIRCLE('',#9009,1.05);
#3636=CIRCLE('',#9011,0.9);
#3637=CIRCLE('',#9015,0.895);
#3638=CIRCLE('',#9016,0.605);
#3639=CIRCLE('',#9019,0.895);
#3640=CIRCLE('',#9020,0.605);
#3641=CIRCLE('',#9023,0.895);
#3642=CIRCLE('',#9024,0.605);
#3643=CIRCLE('',#9026,0.895);
#3644=CIRCLE('',#9028,0.605);
#3645=CIRCLE('',#9042,0.1954);
#3646=CIRCLE('',#9044,0.3);
#3647=CIRCLE('',#9046,0.35);
#3648=CIRCLE('',#9048,0.35);
#3649=CIRCLE('',#9050,0.32);
#3650=CIRCLE('',#9052,0.22);
#3651=CIRCLE('',#9054,0.1954);
#3652=CIRCLE('',#9066,0.25);
#3653=CIRCLE('',#9067,0.21);
#3654=CIRCLE('',#9069,0.25);
#3655=CIRCLE('',#9072,0.375);
#3656=CIRCLE('',#9074,0.425);
#3657=CIRCLE('',#9076,0.425);
#3658=CIRCLE('',#9078,0.395);
#3659=CIRCLE('',#9080,0.27);
#3660=CIRCLE('',#9082,0.24505);
#3661=CIRCLE('',#9084,0.24505);
#3662=CIRCLE('',#9157,0.4);
#3663=CIRCLE('',#9158,0.4);
#3664=CIRCLE('',#9160,0.225);
#3665=CIRCLE('',#9162,0.9);
#3666=CIRCLE('',#9163,0.9);
#3667=CIRCLE('',#9165,0.99);
#3668=CIRCLE('',#9167,0.99);
#3669=CIRCLE('',#9169,0.99);
#3670=CIRCLE('',#9171,0.225);
#3671=CIRCLE('',#9173,0.99);
#3672=CIRCLE('',#9178,0.05);
#3673=CIRCLE('',#9179,0.9);
#3674=CIRCLE('',#9182,0.165);
#3675=CIRCLE('',#9183,0.165);
#3676=CIRCLE('',#9186,0.4);
#3677=CIRCLE('',#9187,0.4);
#3678=CIRCLE('',#9192,0.3);
#3679=CIRCLE('',#9194,0.35);
#3680=CIRCLE('',#9196,0.35);
#3681=CIRCLE('',#9198,0.32);
#3682=CIRCLE('',#9200,0.22);
#3683=CIRCLE('',#9202,0.1954);
#3684=CIRCLE('',#9204,0.1954);
#3685=CIRCLE('',#9206,0.16);
#3686=CIRCLE('',#9218,0.305);
#3687=CIRCLE('',#9219,0.305);
#3688=CIRCLE('',#9221,0.305);
#3689=CIRCLE('',#9222,0.305);
#3690=CIRCLE('',#9224,0.165);
#3691=CIRCLE('',#9226,0.165);
#3692=CIRCLE('',#9227,0.165);
#3693=CIRCLE('',#9228,0.165);
#3694=CIRCLE('',#9231,0.4);
#3695=CIRCLE('',#9232,0.4);
#3696=CIRCLE('',#9252,0.17);
#3697=CIRCLE('',#9254,0.1954);
#3698=CIRCLE('',#9256,0.1954);
#3699=CIRCLE('',#9258,0.125);
#3700=CIRCLE('',#9263,0.45);
#3701=CIRCLE('',#9265,0.5);
#3702=CIRCLE('',#9267,0.5);
#3703=CIRCLE('',#9269,0.3);
#3704=CIRCLE('',#9271,0.3);
#3705=CIRCLE('',#9273,0.21);
#3706=CIRCLE('',#9277,0.32);
#3707=CIRCLE('',#9278,0.32);
#3708=CIRCLE('',#9280,0.6);
#3709=CIRCLE('',#9281,0.6);
#3710=CIRCLE('',#9286,0.08);
#3711=CIRCLE('',#9287,0.04);
#3712=CIRCLE('',#9289,0.08);
#3713=CIRCLE('',#9292,0.08);
#3714=CIRCLE('',#9293,0.08);
#3715=CIRCLE('',#9297,0.3);
#3716=CIRCLE('',#9298,0.3);
#3717=CIRCLE('',#9301,0.6);
#3718=CIRCLE('',#9302,0.6);
#3719=CIRCLE('',#9307,0.3);
#3720=CIRCLE('',#9308,0.3);
#3721=CIRCLE('',#9311,0.6);
#3722=CIRCLE('',#9312,0.6);
#3723=CIRCLE('',#9317,0.325);
#3724=CIRCLE('',#9318,0.325);
#3725=CIRCLE('',#9320,0.325);
#3726=CIRCLE('',#9321,0.325);
#3727=CIRCLE('',#9323,0.31);
#3728=CIRCLE('',#9324,0.31);
#3729=CIRCLE('',#9338,0.32);
#3730=CIRCLE('',#9339,0.32);
#3731=CIRCLE('',#9341,0.6);
#3732=CIRCLE('',#9342,0.6);
#3733=CIRCLE('',#9347,0.475);
#3734=CIRCLE('',#9349,0.475);
#3735=CIRCLE('',#9354,0.25175);
#3736=CIRCLE('',#9355,0.25175);
#3737=VERTEX_POINT('',#11924);
#3738=VERTEX_POINT('',#11926);
#3739=VERTEX_POINT('',#11931);
#3740=VERTEX_POINT('',#11933);
#3741=VERTEX_POINT('',#11938);
#3742=VERTEX_POINT('',#11939);
#3743=VERTEX_POINT('',#11943);
#3744=VERTEX_POINT('',#11947);
#3745=VERTEX_POINT('',#11951);
#3746=VERTEX_POINT('',#11953);
#3747=VERTEX_POINT('',#11956);
#3748=VERTEX_POINT('',#11958);
#3749=VERTEX_POINT('',#11960);
#3750=VERTEX_POINT('',#11962);
#3751=VERTEX_POINT('',#11964);
#3752=VERTEX_POINT('',#11966);
#3753=VERTEX_POINT('',#11971);
#3754=VERTEX_POINT('',#11985);
#3755=VERTEX_POINT('',#11991);
#3756=VERTEX_POINT('',#11993);
#3757=VERTEX_POINT('',#11999);
#3758=VERTEX_POINT('',#12001);
#3759=VERTEX_POINT('',#12006);
#3760=VERTEX_POINT('',#12008);
#3761=VERTEX_POINT('',#12012);
#3762=VERTEX_POINT('',#12014);
#3763=VERTEX_POINT('',#12018);
#3764=VERTEX_POINT('',#12020);
#3765=VERTEX_POINT('',#12024);
#3766=VERTEX_POINT('',#12026);
#3767=VERTEX_POINT('',#12030);
#3768=VERTEX_POINT('',#12032);
#3769=VERTEX_POINT('',#12037);
#3770=VERTEX_POINT('',#12038);
#3771=VERTEX_POINT('',#12040);
#3772=VERTEX_POINT('',#12042);
#3773=VERTEX_POINT('',#12046);
#3774=VERTEX_POINT('',#12048);
#3775=VERTEX_POINT('',#12052);
#3776=VERTEX_POINT('',#12054);
#3777=VERTEX_POINT('',#12064);
#3778=VERTEX_POINT('',#12066);
#3779=VERTEX_POINT('',#12070);
#3780=VERTEX_POINT('',#12071);
#3781=VERTEX_POINT('',#12073);
#3782=VERTEX_POINT('',#12075);
#3783=VERTEX_POINT('',#12080);
#3784=VERTEX_POINT('',#12085);
#3785=VERTEX_POINT('',#12087);
#3786=VERTEX_POINT('',#12091);
#3787=VERTEX_POINT('',#12094);
#3788=VERTEX_POINT('',#12099);
#3789=VERTEX_POINT('',#12103);
#3790=VERTEX_POINT('',#12106);
#3791=VERTEX_POINT('',#12107);
#3792=VERTEX_POINT('',#12109);
#3793=VERTEX_POINT('',#12111);
#3794=VERTEX_POINT('',#12113);
#3795=VERTEX_POINT('',#12115);
#3796=VERTEX_POINT('',#12119);
#3797=VERTEX_POINT('',#12120);
#3798=VERTEX_POINT('',#12122);
#3799=VERTEX_POINT('',#12124);
#3800=VERTEX_POINT('',#12128);
#3801=VERTEX_POINT('',#12131);
#3802=VERTEX_POINT('',#12135);
#3803=VERTEX_POINT('',#12139);
#3804=VERTEX_POINT('',#12145);
#3805=VERTEX_POINT('',#12147);
#3806=VERTEX_POINT('',#12151);
#3807=VERTEX_POINT('',#12155);
#3808=VERTEX_POINT('',#12156);
#3809=VERTEX_POINT('',#12158);
#3810=VERTEX_POINT('',#12160);
#3811=VERTEX_POINT('',#12162);
#3812=VERTEX_POINT('',#12164);
#3813=VERTEX_POINT('',#12167);
#3814=VERTEX_POINT('',#12173);
#3815=VERTEX_POINT('',#12186);
#3816=VERTEX_POINT('',#12190);
#3817=VERTEX_POINT('',#12196);
#3818=VERTEX_POINT('',#12198);
#3819=VERTEX_POINT('',#12201);
#3820=VERTEX_POINT('',#12205);
#3821=VERTEX_POINT('',#12209);
#3822=VERTEX_POINT('',#12212);
#3823=VERTEX_POINT('',#12218);
#3824=VERTEX_POINT('',#12220);
#3825=VERTEX_POINT('',#12225);
#3826=VERTEX_POINT('',#12227);
#3827=VERTEX_POINT('',#12232);
#3828=VERTEX_POINT('',#12233);
#3829=VERTEX_POINT('',#12237);
#3830=VERTEX_POINT('',#12241);
#3831=VERTEX_POINT('',#12245);
#3832=VERTEX_POINT('',#12246);
#3833=VERTEX_POINT('',#12248);
#3834=VERTEX_POINT('',#12250);
#3835=VERTEX_POINT('',#12252);
#3836=VERTEX_POINT('',#12254);
#3837=VERTEX_POINT('',#12256);
#3838=VERTEX_POINT('',#12258);
#3839=VERTEX_POINT('',#12261);
#3840=VERTEX_POINT('',#12282);
#3841=VERTEX_POINT('',#12286);
#3842=VERTEX_POINT('',#12290);
#3843=VERTEX_POINT('',#12292);
#3844=VERTEX_POINT('',#12297);
#3845=VERTEX_POINT('',#12299);
#3846=VERTEX_POINT('',#12303);
#3847=VERTEX_POINT('',#12305);
#3848=VERTEX_POINT('',#12309);
#3849=VERTEX_POINT('',#12311);
#3850=VERTEX_POINT('',#12315);
#3851=VERTEX_POINT('',#12317);
#3852=VERTEX_POINT('',#12321);
#3853=VERTEX_POINT('',#12325);
#3854=VERTEX_POINT('',#12326);
#3855=VERTEX_POINT('',#12328);
#3856=VERTEX_POINT('',#12330);
#3857=VERTEX_POINT('',#12334);
#3858=VERTEX_POINT('',#12336);
#3859=VERTEX_POINT('',#12340);
#3860=VERTEX_POINT('',#12342);
#3861=VERTEX_POINT('',#12352);
#3862=VERTEX_POINT('',#12354);
#3863=VERTEX_POINT('',#12358);
#3864=VERTEX_POINT('',#12359);
#3865=VERTEX_POINT('',#12361);
#3866=VERTEX_POINT('',#12363);
#3867=VERTEX_POINT('',#12368);
#3868=VERTEX_POINT('',#12373);
#3869=VERTEX_POINT('',#12375);
#3870=VERTEX_POINT('',#12379);
#3871=VERTEX_POINT('',#12382);
#3872=VERTEX_POINT('',#12387);
#3873=VERTEX_POINT('',#12391);
#3874=VERTEX_POINT('',#12394);
#3875=VERTEX_POINT('',#12395);
#3876=VERTEX_POINT('',#12397);
#3877=VERTEX_POINT('',#12399);
#3878=VERTEX_POINT('',#12401);
#3879=VERTEX_POINT('',#12403);
#3880=VERTEX_POINT('',#12407);
#3881=VERTEX_POINT('',#12408);
#3882=VERTEX_POINT('',#12410);
#3883=VERTEX_POINT('',#12412);
#3884=VERTEX_POINT('',#12416);
#3885=VERTEX_POINT('',#12419);
#3886=VERTEX_POINT('',#12423);
#3887=VERTEX_POINT('',#12427);
#3888=VERTEX_POINT('',#12433);
#3889=VERTEX_POINT('',#12435);
#3890=VERTEX_POINT('',#12439);
#3891=VERTEX_POINT('',#12443);
#3892=VERTEX_POINT('',#12444);
#3893=VERTEX_POINT('',#12446);
#3894=VERTEX_POINT('',#12448);
#3895=VERTEX_POINT('',#12450);
#3896=VERTEX_POINT('',#12452);
#3897=VERTEX_POINT('',#12455);
#3898=VERTEX_POINT('',#12461);
#3899=VERTEX_POINT('',#12474);
#3900=VERTEX_POINT('',#12478);
#3901=VERTEX_POINT('',#12484);
#3902=VERTEX_POINT('',#12486);
#3903=VERTEX_POINT('',#12489);
#3904=VERTEX_POINT('',#12493);
#3905=VERTEX_POINT('',#12497);
#3906=VERTEX_POINT('',#12500);
#3907=VERTEX_POINT('',#12506);
#3908=VERTEX_POINT('',#12508);
#3909=VERTEX_POINT('',#12512);
#3910=VERTEX_POINT('',#12514);
#3911=VERTEX_POINT('',#12521);
#3912=VERTEX_POINT('',#12523);
#3913=VERTEX_POINT('',#12527);
#3914=VERTEX_POINT('',#12529);
#3915=VERTEX_POINT('',#12536);
#3916=VERTEX_POINT('',#12538);
#3917=VERTEX_POINT('',#12542);
#3918=VERTEX_POINT('',#12544);
#3919=VERTEX_POINT('',#12551);
#3920=VERTEX_POINT('',#12553);
#3921=VERTEX_POINT('',#12557);
#3922=VERTEX_POINT('',#12560);
#3923=VERTEX_POINT('',#12562);
#3924=VERTEX_POINT('',#12566);
#3925=VERTEX_POINT('',#12569);
#3926=VERTEX_POINT('',#12573);
#3927=VERTEX_POINT('',#12577);
#3928=VERTEX_POINT('',#12579);
#3929=VERTEX_POINT('',#12583);
#3930=VERTEX_POINT('',#12586);
#3931=VERTEX_POINT('',#12588);
#3932=VERTEX_POINT('',#12592);
#3933=VERTEX_POINT('',#12595);
#3934=VERTEX_POINT('',#12599);
#3935=VERTEX_POINT('',#12603);
#3936=VERTEX_POINT('',#12604);
#3937=VERTEX_POINT('',#12606);
#3938=VERTEX_POINT('',#12608);
#3939=VERTEX_POINT('',#12612);
#3940=VERTEX_POINT('',#12614);
#3941=VERTEX_POINT('',#12618);
#3942=VERTEX_POINT('',#12620);
#3943=VERTEX_POINT('',#12630);
#3944=VERTEX_POINT('',#12633);
#3945=VERTEX_POINT('',#12637);
#3946=VERTEX_POINT('',#12641);
#3947=VERTEX_POINT('',#12645);
#3948=VERTEX_POINT('',#12648);
#3949=VERTEX_POINT('',#12652);
#3950=VERTEX_POINT('',#12656);
#3951=VERTEX_POINT('',#12661);
#3952=VERTEX_POINT('',#12662);
#3953=VERTEX_POINT('',#12664);
#3954=VERTEX_POINT('',#12666);
#3955=VERTEX_POINT('',#12670);
#3956=VERTEX_POINT('',#12672);
#3957=VERTEX_POINT('',#12676);
#3958=VERTEX_POINT('',#12678);
#3959=VERTEX_POINT('',#12682);
#3960=VERTEX_POINT('',#12684);
#3961=VERTEX_POINT('',#12688);
#3962=VERTEX_POINT('',#12690);
#3963=VERTEX_POINT('',#12701);
#3964=VERTEX_POINT('',#12703);
#3965=VERTEX_POINT('',#12707);
#3966=VERTEX_POINT('',#12710);
#3967=VERTEX_POINT('',#12711);
#3968=VERTEX_POINT('',#12713);
#3969=VERTEX_POINT('',#12715);
#3970=VERTEX_POINT('',#12717);
#3971=VERTEX_POINT('',#12719);
#3972=VERTEX_POINT('',#12722);
#3973=VERTEX_POINT('',#12725);
#3974=VERTEX_POINT('',#12726);
#3975=VERTEX_POINT('',#12728);
#3976=VERTEX_POINT('',#12730);
#3977=VERTEX_POINT('',#12732);
#3978=VERTEX_POINT('',#12734);
#3979=VERTEX_POINT('',#12737);
#3980=VERTEX_POINT('',#12752);
#3981=VERTEX_POINT('',#12755);
#3982=VERTEX_POINT('',#12759);
#3983=VERTEX_POINT('',#12764);
#3984=VERTEX_POINT('',#12768);
#3985=VERTEX_POINT('',#12774);
#3986=VERTEX_POINT('',#12776);
#3987=VERTEX_POINT('',#12779);
#3988=VERTEX_POINT('',#12783);
#3989=VERTEX_POINT('',#12786);
#3990=VERTEX_POINT('',#12790);
#3991=VERTEX_POINT('',#12798);
#3992=VERTEX_POINT('',#12803);
#3993=VERTEX_POINT('',#12805);
#3994=VERTEX_POINT('',#12809);
#3995=VERTEX_POINT('',#12812);
#3996=VERTEX_POINT('',#12815);
#3997=VERTEX_POINT('',#12819);
#3998=VERTEX_POINT('',#12823);
#3999=VERTEX_POINT('',#12825);
#4000=VERTEX_POINT('',#12832);
#4001=VERTEX_POINT('',#12837);
#4002=VERTEX_POINT('',#12839);
#4003=VERTEX_POINT('',#12846);
#4004=VERTEX_POINT('',#12848);
#4005=VERTEX_POINT('',#12852);
#4006=VERTEX_POINT('',#12856);
#4007=VERTEX_POINT('',#12859);
#4008=VERTEX_POINT('',#12865);
#4009=VERTEX_POINT('',#12866);
#4010=VERTEX_POINT('',#12870);
#4011=VERTEX_POINT('',#12874);
#4012=VERTEX_POINT('',#12877);
#4013=VERTEX_POINT('',#12881);
#4014=VERTEX_POINT('',#12885);
#4015=VERTEX_POINT('',#12893);
#4016=VERTEX_POINT('',#12895);
#4017=VERTEX_POINT('',#12897);
#4018=VERTEX_POINT('',#12901);
#4019=VERTEX_POINT('',#12905);
#4020=VERTEX_POINT('',#12909);
#4021=VERTEX_POINT('',#12913);
#4022=VERTEX_POINT('',#12928);
#4023=VERTEX_POINT('',#12930);
#4024=VERTEX_POINT('',#12942);
#4025=VERTEX_POINT('',#12944);
#4026=VERTEX_POINT('',#12948);
#4027=VERTEX_POINT('',#12950);
#4028=VERTEX_POINT('',#12954);
#4029=VERTEX_POINT('',#12956);
#4030=VERTEX_POINT('',#12960);
#4031=VERTEX_POINT('',#12962);
#4032=VERTEX_POINT('',#12966);
#4033=VERTEX_POINT('',#12968);
#4034=VERTEX_POINT('',#12972);
#4035=VERTEX_POINT('',#12974);
#4036=VERTEX_POINT('',#12978);
#4037=VERTEX_POINT('',#12980);
#4038=VERTEX_POINT('',#12984);
#4039=VERTEX_POINT('',#12986);
#4040=VERTEX_POINT('',#12990);
#4041=VERTEX_POINT('',#12992);
#4042=VERTEX_POINT('',#12996);
#4043=VERTEX_POINT('',#12998);
#4044=VERTEX_POINT('',#13002);
#4045=VERTEX_POINT('',#13004);
#4046=VERTEX_POINT('',#13008);
#4047=VERTEX_POINT('',#13010);
#4048=VERTEX_POINT('',#13014);
#4049=VERTEX_POINT('',#13016);
#4050=VERTEX_POINT('',#13020);
#4051=VERTEX_POINT('',#13021);
#4052=VERTEX_POINT('',#13023);
#4053=VERTEX_POINT('',#13025);
#4054=VERTEX_POINT('',#13029);
#4055=VERTEX_POINT('',#13030);
#4056=VERTEX_POINT('',#13032);
#4057=VERTEX_POINT('',#13034);
#4058=VERTEX_POINT('',#13045);
#4059=VERTEX_POINT('',#13047);
#4060=VERTEX_POINT('',#13051);
#4061=VERTEX_POINT('',#13053);
#4062=VERTEX_POINT('',#13057);
#4063=VERTEX_POINT('',#13059);
#4064=VERTEX_POINT('',#13063);
#4065=VERTEX_POINT('',#13065);
#4066=VERTEX_POINT('',#13069);
#4067=VERTEX_POINT('',#13071);
#4068=VERTEX_POINT('',#13075);
#4069=VERTEX_POINT('',#13076);
#4070=VERTEX_POINT('',#13078);
#4071=VERTEX_POINT('',#13080);
#4072=VERTEX_POINT('',#13084);
#4073=VERTEX_POINT('',#13085);
#4074=VERTEX_POINT('',#13087);
#4075=VERTEX_POINT('',#13089);
#4076=VERTEX_POINT('',#13100);
#4077=VERTEX_POINT('',#13101);
#4078=VERTEX_POINT('',#13103);
#4079=VERTEX_POINT('',#13105);
#4080=VERTEX_POINT('',#13109);
#4081=VERTEX_POINT('',#13111);
#4082=VERTEX_POINT('',#13115);
#4083=VERTEX_POINT('',#13117);
#4084=VERTEX_POINT('',#13127);
#4085=VERTEX_POINT('',#13129);
#4086=VERTEX_POINT('',#13133);
#4087=VERTEX_POINT('',#13135);
#4088=VERTEX_POINT('',#13139);
#4089=VERTEX_POINT('',#13141);
#4090=VERTEX_POINT('',#13145);
#4091=VERTEX_POINT('',#13147);
#4092=VERTEX_POINT('',#13151);
#4093=VERTEX_POINT('',#13153);
#4094=VERTEX_POINT('',#13157);
#4095=VERTEX_POINT('',#13159);
#4096=VERTEX_POINT('',#13166);
#4097=VERTEX_POINT('',#13168);
#4098=VERTEX_POINT('',#13172);
#4099=VERTEX_POINT('',#13174);
#4100=VERTEX_POINT('',#13178);
#4101=VERTEX_POINT('',#13180);
#4102=VERTEX_POINT('',#13184);
#4103=VERTEX_POINT('',#13186);
#4104=VERTEX_POINT('',#13190);
#4105=VERTEX_POINT('',#13192);
#4106=VERTEX_POINT('',#13196);
#4107=VERTEX_POINT('',#13198);
#4108=VERTEX_POINT('',#13205);
#4109=VERTEX_POINT('',#13207);
#4110=VERTEX_POINT('',#13211);
#4111=VERTEX_POINT('',#13213);
#4112=VERTEX_POINT('',#13217);
#4113=VERTEX_POINT('',#13219);
#4114=VERTEX_POINT('',#13223);
#4115=VERTEX_POINT('',#13225);
#4116=VERTEX_POINT('',#13229);
#4117=VERTEX_POINT('',#13231);
#4118=VERTEX_POINT('',#13235);
#4119=VERTEX_POINT('',#13237);
#4120=VERTEX_POINT('',#13244);
#4121=VERTEX_POINT('',#13246);
#4122=VERTEX_POINT('',#13250);
#4123=VERTEX_POINT('',#13252);
#4124=VERTEX_POINT('',#13256);
#4125=VERTEX_POINT('',#13258);
#4126=VERTEX_POINT('',#13262);
#4127=VERTEX_POINT('',#13264);
#4128=VERTEX_POINT('',#13268);
#4129=VERTEX_POINT('',#13270);
#4130=VERTEX_POINT('',#13274);
#4131=VERTEX_POINT('',#13276);
#4132=VERTEX_POINT('',#13284);
#4133=VERTEX_POINT('',#13285);
#4134=VERTEX_POINT('',#13287);
#4135=VERTEX_POINT('',#13289);
#4136=VERTEX_POINT('',#13293);
#4137=VERTEX_POINT('',#13295);
#4138=VERTEX_POINT('',#13299);
#4139=VERTEX_POINT('',#13301);
#4140=VERTEX_POINT('',#13309);
#4141=VERTEX_POINT('',#13311);
#4142=VERTEX_POINT('',#13314);
#4143=VERTEX_POINT('',#13318);
#4144=VERTEX_POINT('',#13321);
#4145=VERTEX_POINT('',#13325);
#4146=VERTEX_POINT('',#13328);
#4147=VERTEX_POINT('',#13332);
#4148=VERTEX_POINT('',#13335);
#4149=VERTEX_POINT('',#13339);
#4150=VERTEX_POINT('',#13342);
#4151=VERTEX_POINT('',#13346);
#4152=VERTEX_POINT('',#13352);
#4153=VERTEX_POINT('',#13353);
#4154=VERTEX_POINT('',#13355);
#4155=VERTEX_POINT('',#13357);
#4156=VERTEX_POINT('',#13361);
#4157=VERTEX_POINT('',#13363);
#4158=VERTEX_POINT('',#13367);
#4159=VERTEX_POINT('',#13369);
#4160=VERTEX_POINT('',#13376);
#4161=VERTEX_POINT('',#13378);
#4162=VERTEX_POINT('',#13381);
#4163=VERTEX_POINT('',#13385);
#4164=VERTEX_POINT('',#13393);
#4165=VERTEX_POINT('',#13394);
#4166=VERTEX_POINT('',#13396);
#4167=VERTEX_POINT('',#13398);
#4168=VERTEX_POINT('',#13402);
#4169=VERTEX_POINT('',#13404);
#4170=VERTEX_POINT('',#13408);
#4171=VERTEX_POINT('',#13410);
#4172=VERTEX_POINT('',#13414);
#4173=VERTEX_POINT('',#13416);
#4174=VERTEX_POINT('',#13420);
#4175=VERTEX_POINT('',#13422);
#4176=VERTEX_POINT('',#13431);
#4177=VERTEX_POINT('',#13434);
#4178=VERTEX_POINT('',#13437);
#4179=VERTEX_POINT('',#13441);
#4180=VERTEX_POINT('',#13445);
#4181=VERTEX_POINT('',#13449);
#4182=VERTEX_POINT('',#13452);
#4183=VERTEX_POINT('',#13459);
#4184=VERTEX_POINT('',#13460);
#4185=VERTEX_POINT('',#13462);
#4186=VERTEX_POINT('',#13464);
#4187=VERTEX_POINT('',#13468);
#4188=VERTEX_POINT('',#13470);
#4189=VERTEX_POINT('',#13474);
#4190=VERTEX_POINT('',#13476);
#4191=VERTEX_POINT('',#13480);
#4192=VERTEX_POINT('',#13482);
#4193=VERTEX_POINT('',#13486);
#4194=VERTEX_POINT('',#13488);
#4195=VERTEX_POINT('',#13497);
#4196=VERTEX_POINT('',#13499);
#4197=VERTEX_POINT('',#13502);
#4198=VERTEX_POINT('',#13507);
#4199=VERTEX_POINT('',#13510);
#4200=VERTEX_POINT('',#13514);
#4201=VERTEX_POINT('',#13518);
#4202=VERTEX_POINT('',#13522);
#4203=VERTEX_POINT('',#13525);
#4204=VERTEX_POINT('',#13529);
#4205=VERTEX_POINT('',#13605);
#4206=VERTEX_POINT('',#13607);
#4207=VERTEX_POINT('',#13611);
#4208=VERTEX_POINT('',#13614);
#4209=VERTEX_POINT('',#13616);
#4210=VERTEX_POINT('',#13620);
#4211=VERTEX_POINT('',#13623);
#4212=VERTEX_POINT('',#13626);
#4213=VERTEX_POINT('',#13630);
#4214=VERTEX_POINT('',#13634);
#4215=VERTEX_POINT('',#13641);
#4216=VERTEX_POINT('',#13646);
#4217=VERTEX_POINT('',#13648);
#4218=VERTEX_POINT('',#13653);
#4219=VERTEX_POINT('',#13655);
#4220=VERTEX_POINT('',#13662);
#4221=VERTEX_POINT('',#13665);
#4222=VERTEX_POINT('',#13669);
#4223=VERTEX_POINT('',#13673);
#4224=VERTEX_POINT('',#13677);
#4225=VERTEX_POINT('',#13680);
#4226=VERTEX_POINT('',#13684);
#4227=VERTEX_POINT('',#13688);
#4228=VERTEX_POINT('',#13693);
#4229=VERTEX_POINT('',#13694);
#4230=VERTEX_POINT('',#13696);
#4231=VERTEX_POINT('',#13698);
#4232=VERTEX_POINT('',#13702);
#4233=VERTEX_POINT('',#13704);
#4234=VERTEX_POINT('',#13708);
#4235=VERTEX_POINT('',#13710);
#4236=VERTEX_POINT('',#13714);
#4237=VERTEX_POINT('',#13716);
#4238=VERTEX_POINT('',#13720);
#4239=VERTEX_POINT('',#13722);
#4240=VERTEX_POINT('',#13732);
#4241=VERTEX_POINT('',#13734);
#4242=VERTEX_POINT('',#13738);
#4243=VERTEX_POINT('',#13740);
#4244=VERTEX_POINT('',#13744);
#4245=VERTEX_POINT('',#13745);
#4246=VERTEX_POINT('',#13749);
#4247=VERTEX_POINT('',#13760);
#4248=VERTEX_POINT('',#13762);
#4249=VERTEX_POINT('',#13765);
#4250=VERTEX_POINT('',#13780);
#4251=VERTEX_POINT('',#13782);
#4252=VERTEX_POINT('',#13786);
#4253=VERTEX_POINT('',#13787);
#4254=VERTEX_POINT('',#13789);
#4255=VERTEX_POINT('',#13791);
#4256=VERTEX_POINT('',#13795);
#4257=VERTEX_POINT('',#13797);
#4258=VERTEX_POINT('',#13801);
#4259=VERTEX_POINT('',#13803);
#4260=VERTEX_POINT('',#13807);
#4261=VERTEX_POINT('',#13809);
#4262=VERTEX_POINT('',#13811);
#4263=VERTEX_POINT('',#13813);
#4264=VERTEX_POINT('',#13817);
#4265=VERTEX_POINT('',#13821);
#4266=VERTEX_POINT('',#13825);
#4267=VERTEX_POINT('',#13827);
#4268=VERTEX_POINT('',#13837);
#4269=VERTEX_POINT('',#13838);
#4270=VERTEX_POINT('',#13840);
#4271=VERTEX_POINT('',#13842);
#4272=VERTEX_POINT('',#13846);
#4273=VERTEX_POINT('',#13848);
#4274=VERTEX_POINT('',#13852);
#4275=VERTEX_POINT('',#13854);
#4276=VERTEX_POINT('',#13858);
#4277=VERTEX_POINT('',#13860);
#4278=VERTEX_POINT('',#13864);
#4279=VERTEX_POINT('',#13866);
#4280=VERTEX_POINT('',#13874);
#4281=VERTEX_POINT('',#13877);
#4282=VERTEX_POINT('',#13881);
#4283=VERTEX_POINT('',#13885);
#4284=VERTEX_POINT('',#13891);
#4285=VERTEX_POINT('',#13892);
#4286=VERTEX_POINT('',#13903);
#4287=VERTEX_POINT('',#13939);
#4288=VERTEX_POINT('',#13969);
#4289=VERTEX_POINT('',#13972);
#4290=VERTEX_POINT('',#13976);
#4291=VERTEX_POINT('',#13980);
#4292=VERTEX_POINT('',#13983);
#4293=VERTEX_POINT('',#13988);
#4294=VERTEX_POINT('',#13994);
#4295=VERTEX_POINT('',#13996);
#4296=VERTEX_POINT('',#14000);
#4297=VERTEX_POINT('',#14002);
#4298=VERTEX_POINT('',#14009);
#4299=VERTEX_POINT('',#14012);
#4300=VERTEX_POINT('',#14013);
#4301=VERTEX_POINT('',#14067);
#4302=VERTEX_POINT('',#14068);
#4303=VERTEX_POINT('',#14072);
#4304=VERTEX_POINT('',#14074);
#4305=VERTEX_POINT('',#14078);
#4306=VERTEX_POINT('',#14085);
#4307=VERTEX_POINT('',#14087);
#4308=VERTEX_POINT('',#14092);
#4309=VERTEX_POINT('',#14094);
#4310=VERTEX_POINT('',#14101);
#4311=VERTEX_POINT('',#14103);
#4312=VERTEX_POINT('',#14108);
#4313=VERTEX_POINT('',#14110);
#4314=VERTEX_POINT('',#14117);
#4315=VERTEX_POINT('',#14119);
#4316=VERTEX_POINT('',#14123);
#4317=VERTEX_POINT('',#14125);
#4318=VERTEX_POINT('',#14129);
#4319=VERTEX_POINT('',#14131);
#4320=VERTEX_POINT('',#14135);
#4321=VERTEX_POINT('',#14136);
#4322=VERTEX_POINT('',#14138);
#4323=VERTEX_POINT('',#14140);
#4324=VERTEX_POINT('',#14144);
#4325=VERTEX_POINT('',#14146);
#4326=VERTEX_POINT('',#14150);
#4327=VERTEX_POINT('',#14154);
#4328=VERTEX_POINT('',#14160);
#4329=VERTEX_POINT('',#14161);
#4330=VERTEX_POINT('',#14163);
#4331=VERTEX_POINT('',#14165);
#4332=VERTEX_POINT('',#14169);
#4333=VERTEX_POINT('',#14171);
#4334=VERTEX_POINT('',#14175);
#4335=VERTEX_POINT('',#14177);
#4336=VERTEX_POINT('',#14187);
#4337=VERTEX_POINT('',#14189);
#4338=VERTEX_POINT('',#14193);
#4339=VERTEX_POINT('',#14195);
#4340=VERTEX_POINT('',#14202);
#4341=VERTEX_POINT('',#14203);
#4342=VERTEX_POINT('',#14207);
#4343=VERTEX_POINT('',#14211);
#4344=VERTEX_POINT('',#14214);
#4345=VERTEX_POINT('',#14218);
#4346=VERTEX_POINT('',#14222);
#4347=VERTEX_POINT('',#14230);
#4348=VERTEX_POINT('',#14232);
#4349=VERTEX_POINT('',#14234);
#4350=VERTEX_POINT('',#14238);
#4351=VERTEX_POINT('',#14242);
#4352=VERTEX_POINT('',#14246);
#4353=VERTEX_POINT('',#14250);
#4354=VERTEX_POINT('',#14265);
#4355=VERTEX_POINT('',#14267);
#4356=EDGE_CURVE('',#3737,#3737,#3368,.T.);
#4357=EDGE_CURVE('',#3737,#3738,#2278,.T.);
#4358=EDGE_CURVE('',#3738,#3738,#3369,.T.);
#4359=EDGE_CURVE('',#3739,#3739,#3370,.T.);
#4360=EDGE_CURVE('',#3739,#3740,#2279,.T.);
#4361=EDGE_CURVE('',#3740,#3740,#3371,.T.);
#4362=EDGE_CURVE('',#3741,#3742,#2280,.T.);
#4363=EDGE_CURVE('',#3741,#3742,#3372,.T.);
#4364=EDGE_CURVE('',#3743,#3741,#2281,.T.);
#4365=EDGE_CURVE('',#3743,#3741,#3373,.T.);
#4366=EDGE_CURVE('',#3744,#3743,#825,.T.);
#4367=EDGE_CURVE('',#3741,#3744,#826,.T.);
#4368=EDGE_CURVE('',#3742,#3745,#2282,.T.);
#4369=EDGE_CURVE('',#3746,#3741,#2283,.T.);
#4370=EDGE_CURVE('',#3744,#3746,#827,.T.);
#4371=EDGE_CURVE('',#3747,#3744,#828,.T.);
#4372=EDGE_CURVE('',#3747,#3748,#2284,.T.);
#4373=EDGE_CURVE('',#3749,#3748,#3374,.T.);
#4374=EDGE_CURVE('',#3750,#3749,#2285,.T.);
#4375=EDGE_CURVE('',#3750,#3751,#3375,.T.);
#4376=EDGE_CURVE('',#3752,#3751,#2286,.T.);
#4377=EDGE_CURVE('',#3748,#3752,#3376,.T.);
#4378=EDGE_CURVE('',#3745,#3747,#829,.T.);
#4379=EDGE_CURVE('',#3753,#3747,#830,.T.);
#4380=EDGE_CURVE('',#3742,#3753,#3377,.T.);
#4381=EDGE_CURVE('',#3747,#3742,#831,.T.);
#4382=EDGE_CURVE('',#3751,#3750,#3378,.T.);
#4383=EDGE_CURVE('',#3742,#3753,#2287,.T.);
#4384=EDGE_CURVE('',#3741,#3746,#3379,.T.);
#4385=EDGE_CURVE('',#3742,#3741,#3380,.T.);
#4386=EDGE_CURVE('',#3747,#3754,#2288,.T.);
#4387=EDGE_CURVE('',#3754,#3754,#3381,.T.);
#4388=EDGE_CURVE('',#3745,#3742,#3382,.T.);
#4389=EDGE_CURVE('',#3755,#3749,#3383,.T.);
#4390=EDGE_CURVE('',#3755,#3756,#2289,.T.);
#4391=EDGE_CURVE('',#3756,#3756,#3384,.T.);
#4392=EDGE_CURVE('',#3752,#3755,#3385,.T.);
#4393=EDGE_CURVE('',#3757,#3757,#3386,.T.);
#4394=EDGE_CURVE('',#3757,#3758,#2290,.T.);
#4395=EDGE_CURVE('',#3758,#3758,#3387,.T.);
#4396=EDGE_CURVE('',#3759,#3759,#3388,.T.);
#4397=EDGE_CURVE('',#3759,#3760,#2291,.T.);
#4398=EDGE_CURVE('',#3760,#3760,#3389,.T.);
#4399=EDGE_CURVE('',#3761,#3761,#3390,.T.);
#4400=EDGE_CURVE('',#3761,#3762,#2292,.T.);
#4401=EDGE_CURVE('',#3762,#3762,#3391,.T.);
#4402=EDGE_CURVE('',#3763,#3763,#3392,.T.);
#4403=EDGE_CURVE('',#3763,#3764,#2293,.T.);
#4404=EDGE_CURVE('',#3764,#3764,#3393,.T.);
#4405=EDGE_CURVE('',#3765,#3765,#3394,.T.);
#4406=EDGE_CURVE('',#3765,#3766,#2294,.T.);
#4407=EDGE_CURVE('',#3766,#3766,#3395,.T.);
#4408=EDGE_CURVE('',#3767,#3767,#3396,.T.);
#4409=EDGE_CURVE('',#3767,#3768,#2295,.T.);
#4410=EDGE_CURVE('',#3768,#3768,#3397,.T.);
#4411=EDGE_CURVE('',#3769,#3770,#2296,.T.);
#4412=EDGE_CURVE('',#3770,#3771,#2297,.T.);
#4413=EDGE_CURVE('',#3772,#3771,#2298,.T.);
#4414=EDGE_CURVE('',#3769,#3772,#2299,.T.);
#4415=EDGE_CURVE('',#3773,#3769,#2300,.T.);
#4416=EDGE_CURVE('',#3774,#3772,#2301,.T.);
#4417=EDGE_CURVE('',#3773,#3774,#2302,.T.);
#4418=EDGE_CURVE('',#3775,#3773,#2303,.T.);
#4419=EDGE_CURVE('',#3776,#3774,#2304,.T.);
#4420=EDGE_CURVE('',#3775,#3776,#2305,.T.);
#4421=EDGE_CURVE('',#3770,#3775,#2306,.T.);
#4422=EDGE_CURVE('',#3771,#3776,#2307,.T.);
#4423=EDGE_CURVE('',#3777,#3777,#3398,.T.);
#4424=EDGE_CURVE('',#3777,#3778,#2308,.T.);
#4425=EDGE_CURVE('',#3778,#3778,#3399,.T.);
#4426=EDGE_CURVE('',#3779,#3780,#2309,.T.);
#4427=EDGE_CURVE('',#3781,#3779,#2310,.T.);
#4428=EDGE_CURVE('',#3782,#3781,#2311,.T.);
#4429=EDGE_CURVE('',#3780,#3782,#2312,.T.);
#4430=EDGE_CURVE('',#3781,#3779,#3400,.T.);
#4431=EDGE_CURVE('',#3783,#3783,#3401,.T.);
#4432=EDGE_CURVE('',#3782,#3780,#3402,.T.);
#4433=EDGE_CURVE('',#3784,#3784,#3403,.T.);
#4434=EDGE_CURVE('',#3784,#3785,#2313,.T.);
#4435=EDGE_CURVE('',#3785,#3785,#3404,.T.);
#4436=EDGE_CURVE('',#3786,#3786,#3405,.T.);
#4437=EDGE_CURVE('',#3787,#3787,#3406,.T.);
#4438=EDGE_CURVE('',#3783,#3787,#2314,.T.);
#4439=EDGE_CURVE('',#3786,#3788,#2315,.T.);
#4440=EDGE_CURVE('',#3788,#3788,#3407,.T.);
#4441=EDGE_CURVE('',#3789,#3789,#3408,.T.);
#4442=EDGE_CURVE('',#3790,#3791,#2316,.T.);
#4443=EDGE_CURVE('',#3791,#3792,#2317,.T.);
#4444=EDGE_CURVE('',#3792,#3793,#2318,.T.);
#4445=EDGE_CURVE('',#3794,#3793,#2319,.T.);
#4446=EDGE_CURVE('',#3795,#3794,#2320,.T.);
#4447=EDGE_CURVE('',#3790,#3795,#2321,.T.);
#4448=EDGE_CURVE('',#3796,#3797,#2322,.T.);
#4449=EDGE_CURVE('',#3797,#3798,#2323,.T.);
#4450=EDGE_CURVE('',#3799,#3798,#2324,.T.);
#4451=EDGE_CURVE('',#3796,#3799,#2325,.T.);
#4452=EDGE_CURVE('',#3800,#3793,#2326,.T.);
#4453=EDGE_CURVE('',#3800,#3796,#2327,.T.);
#4454=EDGE_CURVE('',#3801,#3799,#2328,.T.);
#4455=EDGE_CURVE('',#3794,#3801,#2329,.T.);
#4456=EDGE_CURVE('',#3802,#3801,#2330,.T.);
#4457=EDGE_CURVE('',#3795,#3802,#2331,.T.);
#4458=EDGE_CURVE('',#3797,#3803,#2332,.T.);
#4459=EDGE_CURVE('',#3790,#3803,#2333,.T.);
#4460=EDGE_CURVE('',#3798,#3802,#2334,.T.);
#4461=EDGE_CURVE('',#3804,#3803,#2335,.T.);
#4462=EDGE_CURVE('',#3800,#3805,#2336,.T.);
#4463=EDGE_CURVE('',#3805,#3804,#2337,.T.);
#4464=EDGE_CURVE('',#3793,#3806,#2338,.T.);
#4465=EDGE_CURVE('',#3806,#3800,#2339,.T.);
#4466=EDGE_CURVE('',#3807,#3808,#2340,.T.);
#4467=EDGE_CURVE('',#3809,#3807,#2341,.T.);
#4468=EDGE_CURVE('',#3810,#3809,#2342,.T.);
#4469=EDGE_CURVE('',#3811,#3810,#2343,.T.);
#4470=EDGE_CURVE('',#3812,#3811,#2344,.T.);
#4471=EDGE_CURVE('',#3808,#3812,#2345,.T.);
#4472=EDGE_CURVE('',#3813,#3813,#3409,.T.);
#4473=EDGE_CURVE('',#3807,#3792,#2346,.T.);
#4474=EDGE_CURVE('',#3809,#3791,#2347,.T.);
#4475=EDGE_CURVE('',#3814,#3790,#2348,.T.);
#4476=EDGE_CURVE('',#3810,#3814,#2349,.T.);
#4477=EDGE_CURVE('',#3803,#3814,#2350,.T.);
#4478=EDGE_CURVE('',#3811,#3804,#2351,.T.);
#4479=EDGE_CURVE('',#3812,#3805,#2352,.T.);
#4480=EDGE_CURVE('',#3808,#3806,#2353,.T.);
#4481=EDGE_CURVE('',#3789,#3815,#2354,.T.);
#4482=EDGE_CURVE('',#3815,#3815,#3410,.T.);
#4483=EDGE_CURVE('',#3813,#3816,#2355,.T.);
#4484=EDGE_CURVE('',#3816,#3816,#3411,.T.);
#4485=EDGE_CURVE('',#3817,#3817,#3412,.T.);
#4486=EDGE_CURVE('',#3817,#3818,#2356,.T.);
#4487=EDGE_CURVE('',#3819,#3819,#3413,.T.);
#4488=EDGE_CURVE('',#3819,#3817,#2357,.T.);
#4489=EDGE_CURVE('',#3820,#3820,#3414,.T.);
#4490=EDGE_CURVE('',#3820,#3819,#2358,.T.);
#4491=EDGE_CURVE('',#3821,#3821,#3415,.T.);
#4492=EDGE_CURVE('',#3822,#3822,#3416,.T.);
#4493=EDGE_CURVE('',#3822,#3821,#2359,.T.);
#4494=EDGE_CURVE('',#3823,#3823,#3417,.T.);
#4495=EDGE_CURVE('',#3823,#3824,#2360,.T.);
#4496=EDGE_CURVE('',#3824,#3824,#3418,.T.);
#4497=EDGE_CURVE('',#3825,#3825,#3419,.T.);
#4498=EDGE_CURVE('',#3825,#3826,#2361,.T.);
#4499=EDGE_CURVE('',#3826,#3826,#3420,.T.);
#4500=EDGE_CURVE('',#3827,#3828,#2362,.T.);
#4501=EDGE_CURVE('',#3828,#3827,#3421,.T.);
#4502=EDGE_CURVE('',#3828,#3829,#2363,.T.);
#4503=EDGE_CURVE('',#3829,#3828,#3422,.T.);
#4504=EDGE_CURVE('',#3830,#3827,#2364,.T.);
#4505=EDGE_CURVE('',#3827,#3830,#3423,.T.);
#4506=EDGE_CURVE('',#3831,#3832,#2365,.T.);
#4507=EDGE_CURVE('',#3833,#3831,#3424,.T.);
#4508=EDGE_CURVE('',#3834,#3833,#2366,.T.);
#4509=EDGE_CURVE('',#3835,#3834,#3425,.T.);
#4510=EDGE_CURVE('',#3835,#3836,#2367,.T.);
#4511=EDGE_CURVE('',#3837,#3836,#832,.T.);
#4512=EDGE_CURVE('',#3838,#3837,#833,.T.);
#4513=EDGE_CURVE('',#3828,#3838,#2368,.T.);
#4514=EDGE_CURVE('',#3839,#3827,#2369,.T.);
#4515=EDGE_CURVE('',#3836,#3839,#834,.T.);
#4516=EDGE_CURVE('',#3832,#3835,#3426,.T.);
#4517=EDGE_CURVE('',#3829,#3837,#835,.T.);
#4518=EDGE_CURVE('',#3837,#3828,#836,.T.);
#4519=EDGE_CURVE('',#3836,#3830,#837,.T.);
#4520=EDGE_CURVE('',#3827,#3836,#838,.T.);
#4521=EDGE_CURVE('',#3833,#3831,#3427,.T.);
#4522=EDGE_CURVE('',#3828,#3827,#3428,.T.);
#4523=EDGE_CURVE('',#3838,#3828,#3429,.T.);
#4524=EDGE_CURVE('',#3827,#3839,#3430,.T.);
#4525=EDGE_CURVE('',#3836,#3840,#2370,.T.);
#4526=EDGE_CURVE('',#3840,#3840,#3431,.T.);
#4527=EDGE_CURVE('',#3841,#3834,#3432,.T.);
#4528=EDGE_CURVE('',#3832,#3841,#3433,.T.);
#4529=EDGE_CURVE('',#3842,#3842,#3434,.T.);
#4530=EDGE_CURVE('',#3842,#3843,#2371,.T.);
#4531=EDGE_CURVE('',#3843,#3843,#3435,.T.);
#4532=EDGE_CURVE('',#3844,#3844,#3436,.T.);
#4533=EDGE_CURVE('',#3844,#3845,#2372,.T.);
#4534=EDGE_CURVE('',#3845,#3845,#3437,.T.);
#4535=EDGE_CURVE('',#3846,#3846,#3438,.T.);
#4536=EDGE_CURVE('',#3846,#3847,#2373,.T.);
#4537=EDGE_CURVE('',#3847,#3847,#3439,.T.);
#4538=EDGE_CURVE('',#3848,#3848,#3440,.T.);
#4539=EDGE_CURVE('',#3848,#3849,#2374,.T.);
#4540=EDGE_CURVE('',#3849,#3849,#3441,.T.);
#4541=EDGE_CURVE('',#3850,#3850,#3442,.T.);
#4542=EDGE_CURVE('',#3850,#3851,#2375,.T.);
#4543=EDGE_CURVE('',#3851,#3851,#3443,.T.);
#4544=EDGE_CURVE('',#3852,#3852,#3444,.T.);
#4545=EDGE_CURVE('',#3852,#3841,#2376,.T.);
#4546=EDGE_CURVE('',#3853,#3854,#2377,.T.);
#4547=EDGE_CURVE('',#3854,#3855,#2378,.T.);
#4548=EDGE_CURVE('',#3856,#3855,#2379,.T.);
#4549=EDGE_CURVE('',#3853,#3856,#2380,.T.);
#4550=EDGE_CURVE('',#3857,#3853,#2381,.T.);
#4551=EDGE_CURVE('',#3858,#3856,#2382,.T.);
#4552=EDGE_CURVE('',#3857,#3858,#2383,.T.);
#4553=EDGE_CURVE('',#3859,#3857,#2384,.T.);
#4554=EDGE_CURVE('',#3860,#3858,#2385,.T.);
#4555=EDGE_CURVE('',#3859,#3860,#2386,.T.);
#4556=EDGE_CURVE('',#3854,#3859,#2387,.T.);
#4557=EDGE_CURVE('',#3855,#3860,#2388,.T.);
#4558=EDGE_CURVE('',#3861,#3861,#3445,.T.);
#4559=EDGE_CURVE('',#3861,#3862,#2389,.T.);
#4560=EDGE_CURVE('',#3862,#3862,#3446,.T.);
#4561=EDGE_CURVE('',#3863,#3864,#2390,.T.);
#4562=EDGE_CURVE('',#3865,#3863,#2391,.T.);
#4563=EDGE_CURVE('',#3866,#3865,#2392,.T.);
#4564=EDGE_CURVE('',#3864,#3866,#2393,.T.);
#4565=EDGE_CURVE('',#3865,#3863,#3447,.T.);
#4566=EDGE_CURVE('',#3867,#3867,#3448,.T.);
#4567=EDGE_CURVE('',#3866,#3864,#3449,.T.);
#4568=EDGE_CURVE('',#3868,#3868,#3450,.T.);
#4569=EDGE_CURVE('',#3868,#3869,#2394,.T.);
#4570=EDGE_CURVE('',#3869,#3869,#3451,.T.);
#4571=EDGE_CURVE('',#3870,#3870,#3452,.T.);
#4572=EDGE_CURVE('',#3871,#3871,#3453,.T.);
#4573=EDGE_CURVE('',#3867,#3871,#2395,.T.);
#4574=EDGE_CURVE('',#3870,#3872,#2396,.T.);
#4575=EDGE_CURVE('',#3872,#3872,#3454,.T.);
#4576=EDGE_CURVE('',#3873,#3873,#3455,.T.);
#4577=EDGE_CURVE('',#3874,#3875,#2397,.T.);
#4578=EDGE_CURVE('',#3875,#3876,#2398,.T.);
#4579=EDGE_CURVE('',#3876,#3877,#2399,.T.);
#4580=EDGE_CURVE('',#3878,#3877,#2400,.T.);
#4581=EDGE_CURVE('',#3879,#3878,#2401,.T.);
#4582=EDGE_CURVE('',#3874,#3879,#2402,.T.);
#4583=EDGE_CURVE('',#3880,#3881,#2403,.T.);
#4584=EDGE_CURVE('',#3881,#3882,#2404,.T.);
#4585=EDGE_CURVE('',#3883,#3882,#2405,.T.);
#4586=EDGE_CURVE('',#3880,#3883,#2406,.T.);
#4587=EDGE_CURVE('',#3884,#3877,#2407,.T.);
#4588=EDGE_CURVE('',#3884,#3880,#2408,.T.);
#4589=EDGE_CURVE('',#3885,#3883,#2409,.T.);
#4590=EDGE_CURVE('',#3878,#3885,#2410,.T.);
#4591=EDGE_CURVE('',#3886,#3885,#2411,.T.);
#4592=EDGE_CURVE('',#3879,#3886,#2412,.T.);
#4593=EDGE_CURVE('',#3881,#3887,#2413,.T.);
#4594=EDGE_CURVE('',#3874,#3887,#2414,.T.);
#4595=EDGE_CURVE('',#3882,#3886,#2415,.T.);
#4596=EDGE_CURVE('',#3888,#3887,#2416,.T.);
#4597=EDGE_CURVE('',#3884,#3889,#2417,.T.);
#4598=EDGE_CURVE('',#3889,#3888,#2418,.T.);
#4599=EDGE_CURVE('',#3877,#3890,#2419,.T.);
#4600=EDGE_CURVE('',#3890,#3884,#2420,.T.);
#4601=EDGE_CURVE('',#3891,#3892,#2421,.T.);
#4602=EDGE_CURVE('',#3893,#3891,#2422,.T.);
#4603=EDGE_CURVE('',#3894,#3893,#2423,.T.);
#4604=EDGE_CURVE('',#3895,#3894,#2424,.T.);
#4605=EDGE_CURVE('',#3896,#3895,#2425,.T.);
#4606=EDGE_CURVE('',#3892,#3896,#2426,.T.);
#4607=EDGE_CURVE('',#3897,#3897,#3456,.T.);
#4608=EDGE_CURVE('',#3891,#3876,#2427,.T.);
#4609=EDGE_CURVE('',#3893,#3875,#2428,.T.);
#4610=EDGE_CURVE('',#3898,#3874,#2429,.T.);
#4611=EDGE_CURVE('',#3894,#3898,#2430,.T.);
#4612=EDGE_CURVE('',#3887,#3898,#2431,.T.);
#4613=EDGE_CURVE('',#3895,#3888,#2432,.T.);
#4614=EDGE_CURVE('',#3896,#3889,#2433,.T.);
#4615=EDGE_CURVE('',#3892,#3890,#2434,.T.);
#4616=EDGE_CURVE('',#3873,#3899,#2435,.T.);
#4617=EDGE_CURVE('',#3899,#3899,#3457,.T.);
#4618=EDGE_CURVE('',#3897,#3900,#2436,.T.);
#4619=EDGE_CURVE('',#3900,#3900,#3458,.T.);
#4620=EDGE_CURVE('',#3901,#3901,#3459,.T.);
#4621=EDGE_CURVE('',#3901,#3902,#2437,.T.);
#4622=EDGE_CURVE('',#3903,#3903,#3460,.T.);
#4623=EDGE_CURVE('',#3903,#3901,#2438,.T.);
#4624=EDGE_CURVE('',#3904,#3904,#3461,.T.);
#4625=EDGE_CURVE('',#3904,#3903,#2439,.T.);
#4626=EDGE_CURVE('',#3905,#3905,#3462,.T.);
#4627=EDGE_CURVE('',#3906,#3906,#3463,.T.);
#4628=EDGE_CURVE('',#3906,#3905,#2440,.T.);
#4629=EDGE_CURVE('',#3907,#3907,#3464,.T.);
#4630=EDGE_CURVE('',#3907,#3908,#2441,.T.);
#4631=EDGE_CURVE('',#3908,#3908,#3465,.T.);
#4632=EDGE_CURVE('',#3909,#3909,#3466,.T.);
#4633=EDGE_CURVE('',#3909,#3910,#2442,.T.);
#4634=EDGE_CURVE('',#3910,#3910,#3467,.T.);
#4635=EDGE_CURVE('',#3911,#3911,#3468,.T.);
#4636=EDGE_CURVE('',#3911,#3912,#2443,.T.);
#4637=EDGE_CURVE('',#3912,#3912,#3469,.T.);
#4638=EDGE_CURVE('',#3913,#3913,#3470,.T.);
#4639=EDGE_CURVE('',#3913,#3914,#2444,.T.);
#4640=EDGE_CURVE('',#3914,#3914,#3471,.T.);
#4641=EDGE_CURVE('',#3915,#3915,#3472,.T.);
#4642=EDGE_CURVE('',#3915,#3916,#2445,.T.);
#4643=EDGE_CURVE('',#3916,#3916,#3473,.T.);
#4644=EDGE_CURVE('',#3917,#3917,#3474,.T.);
#4645=EDGE_CURVE('',#3917,#3918,#2446,.T.);
#4646=EDGE_CURVE('',#3918,#3918,#3475,.T.);
#4647=EDGE_CURVE('',#3919,#3919,#3476,.T.);
#4648=EDGE_CURVE('',#3919,#3920,#2447,.T.);
#4649=EDGE_CURVE('',#3920,#3920,#3477,.T.);
#4650=EDGE_CURVE('',#3921,#3921,#3478,.T.);
#4651=EDGE_CURVE('',#3922,#3922,#3479,.T.);
#4652=EDGE_CURVE('',#3922,#3923,#2448,.T.);
#4653=EDGE_CURVE('',#3923,#3923,#3480,.T.);
#4654=EDGE_CURVE('',#3924,#3924,#3481,.T.);
#4655=EDGE_CURVE('',#3925,#3925,#3482,.T.);
#4656=EDGE_CURVE('',#3925,#3921,#2449,.T.);
#4657=EDGE_CURVE('',#3926,#3926,#3483,.T.);
#4658=EDGE_CURVE('',#3926,#3924,#2450,.T.);
#4659=EDGE_CURVE('',#3927,#3927,#3484,.T.);
#4660=EDGE_CURVE('',#3927,#3928,#2451,.T.);
#4661=EDGE_CURVE('',#3928,#3928,#3485,.T.);
#4662=EDGE_CURVE('',#3929,#3929,#3486,.T.);
#4663=EDGE_CURVE('',#3930,#3930,#3487,.T.);
#4664=EDGE_CURVE('',#3930,#3931,#2452,.T.);
#4665=EDGE_CURVE('',#3931,#3931,#3488,.T.);
#4666=EDGE_CURVE('',#3932,#3932,#3489,.T.);
#4667=EDGE_CURVE('',#3929,#3933,#2453,.T.);
#4668=EDGE_CURVE('',#3933,#3933,#3490,.T.);
#4669=EDGE_CURVE('',#3932,#3934,#2454,.T.);
#4670=EDGE_CURVE('',#3934,#3934,#3491,.T.);
#4671=EDGE_CURVE('',#3935,#3936,#2455,.T.);
#4672=EDGE_CURVE('',#3936,#3937,#2456,.T.);
#4673=EDGE_CURVE('',#3938,#3937,#2457,.T.);
#4674=EDGE_CURVE('',#3935,#3938,#2458,.T.);
#4675=EDGE_CURVE('',#3939,#3935,#2459,.T.);
#4676=EDGE_CURVE('',#3940,#3938,#2460,.T.);
#4677=EDGE_CURVE('',#3939,#3940,#2461,.T.);
#4678=EDGE_CURVE('',#3941,#3939,#2462,.T.);
#4679=EDGE_CURVE('',#3942,#3940,#2463,.T.);
#4680=EDGE_CURVE('',#3941,#3942,#2464,.T.);
#4681=EDGE_CURVE('',#3936,#3941,#2465,.T.);
#4682=EDGE_CURVE('',#3937,#3942,#2466,.T.);
#4683=EDGE_CURVE('',#3943,#3943,#3492,.T.);
#4684=EDGE_CURVE('',#3944,#3944,#3493,.T.);
#4685=EDGE_CURVE('',#3944,#3943,#2467,.T.);
#4686=EDGE_CURVE('',#3945,#3945,#3494,.T.);
#4687=EDGE_CURVE('',#3945,#3944,#2468,.T.);
#4688=EDGE_CURVE('',#3946,#3946,#3495,.T.);
#4689=EDGE_CURVE('',#3946,#3945,#2469,.T.);
#4690=EDGE_CURVE('',#3947,#3947,#3496,.T.);
#4691=EDGE_CURVE('',#3948,#3948,#3497,.F.);
#4692=EDGE_CURVE('',#3948,#3947,#2470,.T.);
#4693=EDGE_CURVE('',#3949,#3949,#3498,.F.);
#4694=EDGE_CURVE('',#3949,#3948,#2471,.T.);
#4695=EDGE_CURVE('',#3950,#3950,#3499,.T.);
#4696=EDGE_CURVE('',#3950,#3949,#2472,.T.);
#4697=EDGE_CURVE('',#3951,#3952,#2473,.T.);
#4698=EDGE_CURVE('',#3952,#3953,#2474,.T.);
#4699=EDGE_CURVE('',#3953,#3954,#2475,.T.);
#4700=EDGE_CURVE('',#3951,#3954,#2476,.T.);
#4701=EDGE_CURVE('',#3952,#3955,#2477,.T.);
#4702=EDGE_CURVE('',#3955,#3956,#2478,.T.);
#4703=EDGE_CURVE('',#3956,#3953,#2479,.T.);
#4704=EDGE_CURVE('',#3955,#3957,#2480,.T.);
#4705=EDGE_CURVE('',#3957,#3958,#2481,.T.);
#4706=EDGE_CURVE('',#3958,#3956,#2482,.T.);
#4707=EDGE_CURVE('',#3957,#3959,#2483,.T.);
#4708=EDGE_CURVE('',#3959,#3960,#2484,.T.);
#4709=EDGE_CURVE('',#3960,#3958,#2485,.T.);
#4710=EDGE_CURVE('',#3959,#3961,#2486,.T.);
#4711=EDGE_CURVE('',#3961,#3962,#2487,.T.);
#4712=EDGE_CURVE('',#3962,#3960,#2488,.T.);
#4713=EDGE_CURVE('',#3961,#3951,#2489,.T.);
#4714=EDGE_CURVE('',#3954,#3962,#2490,.T.);
#4715=EDGE_CURVE('',#3963,#3963,#3500,.T.);
#4716=EDGE_CURVE('',#3963,#3964,#2491,.T.);
#4717=EDGE_CURVE('',#3964,#3964,#3501,.T.);
#4718=EDGE_CURVE('',#3965,#3965,#3502,.T.);
#4719=EDGE_CURVE('',#3966,#3967,#2492,.T.);
#4720=EDGE_CURVE('',#3967,#3968,#2493,.T.);
#4721=EDGE_CURVE('',#3968,#3969,#2494,.T.);
#4722=EDGE_CURVE('',#3969,#3970,#2495,.T.);
#4723=EDGE_CURVE('',#3970,#3971,#2496,.T.);
#4724=EDGE_CURVE('',#3971,#3966,#2497,.T.);
#4725=EDGE_CURVE('',#3972,#3972,#3503,.T.);
#4726=EDGE_CURVE('',#3973,#3974,#2498,.T.);
#4727=EDGE_CURVE('',#3975,#3973,#2499,.T.);
#4728=EDGE_CURVE('',#3976,#3975,#2500,.T.);
#4729=EDGE_CURVE('',#3977,#3976,#2501,.T.);
#4730=EDGE_CURVE('',#3978,#3977,#2502,.T.);
#4731=EDGE_CURVE('',#3974,#3978,#2503,.T.);
#4732=EDGE_CURVE('',#3979,#3979,#3504,.T.);
#4733=EDGE_CURVE('',#3973,#3966,#2504,.T.);
#4734=EDGE_CURVE('',#3975,#3971,#2505,.T.);
#4735=EDGE_CURVE('',#3976,#3970,#2506,.T.);
#4736=EDGE_CURVE('',#3977,#3969,#2507,.T.);
#4737=EDGE_CURVE('',#3978,#3968,#2508,.T.);
#4738=EDGE_CURVE('',#3974,#3967,#2509,.T.);
#4739=EDGE_CURVE('',#3980,#3980,#3505,.T.);
#4740=EDGE_CURVE('',#3980,#3981,#2510,.T.);
#4741=EDGE_CURVE('',#3981,#3981,#3506,.T.);
#4742=EDGE_CURVE('',#3982,#3982,#3507,.T.);
#4743=EDGE_CURVE('',#3972,#3982,#2511,.T.);
#4744=EDGE_CURVE('',#3983,#3983,#3508,.T.);
#4745=EDGE_CURVE('',#3983,#3979,#2512,.T.);
#4746=EDGE_CURVE('',#3984,#3984,#3509,.T.);
#4747=EDGE_CURVE('',#3984,#3965,#2513,.T.);
#4748=EDGE_CURVE('',#3985,#3985,#3510,.T.);
#4749=EDGE_CURVE('',#3986,#3986,#3511,.T.);
#4750=EDGE_CURVE('',#3987,#3987,#3512,.T.);
#4751=EDGE_CURVE('',#3987,#3985,#2514,.T.);
#4752=EDGE_CURVE('',#3988,#3988,#3513,.T.);
#4753=EDGE_CURVE('',#3989,#3989,#3514,.T.);
#4754=EDGE_CURVE('',#3989,#3988,#2515,.T.);
#4755=EDGE_CURVE('',#3990,#3990,#3515,.T.);
#4756=EDGE_CURVE('',#3990,#3986,#2516,.T.);
#4757=EDGE_CURVE('',#3991,#3991,#3516,.T.);
#4758=EDGE_CURVE('',#3991,#3991,#3517,.T.);
#4759=EDGE_CURVE('',#3992,#3992,#3518,.T.);
#4760=EDGE_CURVE('',#3992,#3993,#2517,.T.);
#4761=EDGE_CURVE('',#3993,#3993,#3519,.T.);
#4762=EDGE_CURVE('',#3994,#3994,#3520,.T.);
#4763=EDGE_CURVE('',#3995,#3995,#3521,.T.);
#4764=EDGE_CURVE('',#3995,#3996,#2518,.T.);
#4765=EDGE_CURVE('',#3996,#3996,#3522,.T.);
#4766=EDGE_CURVE('',#3997,#3997,#3523,.T.);
#4767=EDGE_CURVE('',#3997,#3994,#2519,.T.);
#4768=EDGE_CURVE('',#3998,#3998,#3524,.T.);
#4769=EDGE_CURVE('',#3998,#3999,#2520,.T.);
#4770=EDGE_CURVE('',#3999,#3999,#3525,.T.);
#4771=EDGE_CURVE('',#4000,#4000,#3526,.T.);
#4772=EDGE_CURVE('',#4000,#4000,#3527,.T.);
#4773=EDGE_CURVE('',#4001,#4001,#3528,.T.);
#4774=EDGE_CURVE('',#4001,#4002,#2521,.T.);
#4775=EDGE_CURVE('',#4002,#4002,#3529,.T.);
#4776=EDGE_CURVE('',#4003,#4003,#3530,.T.);
#4777=EDGE_CURVE('',#4003,#4004,#2522,.T.);
#4778=EDGE_CURVE('',#4004,#4004,#3531,.T.);
#4779=EDGE_CURVE('',#4004,#4005,#2523,.T.);
#4780=EDGE_CURVE('',#4005,#4005,#3532,.T.);
#4781=EDGE_CURVE('',#4006,#4006,#3533,.T.);
#4782=EDGE_CURVE('',#4006,#4007,#2524,.T.);
#4783=EDGE_CURVE('',#4007,#4007,#3534,.T.);
#4784=EDGE_CURVE('',#4008,#4009,#19,.T.);
#4785=EDGE_CURVE('',#4010,#4008,#20,.T.);
#4786=EDGE_CURVE('',#4010,#4011,#2525,.T.);
#4787=EDGE_CURVE('',#4011,#4011,#3535,.T.);
#4788=EDGE_CURVE('',#4012,#4010,#21,.T.);
#4789=EDGE_CURVE('',#4013,#4012,#22,.T.);
#4790=EDGE_CURVE('',#4014,#4013,#23,.T.);
#4791=EDGE_CURVE('',#4009,#4014,#24,.T.);
#4792=EDGE_CURVE('',#4015,#4015,#3536,.T.);
#4793=EDGE_CURVE('',#4015,#4016,#2526,.T.);
#4794=EDGE_CURVE('',#4017,#4016,#25,.T.);
#4795=EDGE_CURVE('',#4018,#4017,#26,.T.);
#4796=EDGE_CURVE('',#4019,#4018,#27,.T.);
#4797=EDGE_CURVE('',#4020,#4019,#28,.T.);
#4798=EDGE_CURVE('',#4021,#4020,#29,.T.);
#4799=EDGE_CURVE('',#4016,#4021,#30,.T.);
#4800=EDGE_CURVE('',#4012,#4021,#2527,.T.);
#4801=EDGE_CURVE('',#4013,#4020,#2528,.T.);
#4802=EDGE_CURVE('',#4010,#4016,#2529,.T.);
#4803=EDGE_CURVE('',#4008,#4017,#2530,.T.);
#4804=EDGE_CURVE('',#4022,#4022,#3537,.F.);
#4805=EDGE_CURVE('',#4022,#4023,#2531,.T.);
#4806=EDGE_CURVE('',#4023,#4023,#3538,.F.);
#4807=EDGE_CURVE('',#4009,#4018,#2532,.T.);
#4808=EDGE_CURVE('',#4014,#4019,#2533,.T.);
#4809=EDGE_CURVE('',#4024,#4024,#3539,.T.);
#4810=EDGE_CURVE('',#4024,#4025,#2534,.T.);
#4811=EDGE_CURVE('',#4025,#4025,#3540,.T.);
#4812=EDGE_CURVE('',#4026,#4026,#3541,.T.);
#4813=EDGE_CURVE('',#4026,#4027,#2535,.T.);
#4814=EDGE_CURVE('',#4027,#4027,#3542,.T.);
#4815=EDGE_CURVE('',#4028,#4028,#3543,.T.);
#4816=EDGE_CURVE('',#4028,#4029,#2536,.T.);
#4817=EDGE_CURVE('',#4029,#4029,#3544,.T.);
#4818=EDGE_CURVE('',#4030,#4030,#3545,.T.);
#4819=EDGE_CURVE('',#4030,#4031,#2537,.T.);
#4820=EDGE_CURVE('',#4031,#4031,#3546,.T.);
#4821=EDGE_CURVE('',#4032,#4032,#3547,.T.);
#4822=EDGE_CURVE('',#4032,#4033,#2538,.T.);
#4823=EDGE_CURVE('',#4033,#4033,#3548,.T.);
#4824=EDGE_CURVE('',#4034,#4034,#3549,.T.);
#4825=EDGE_CURVE('',#4034,#4035,#2539,.T.);
#4826=EDGE_CURVE('',#4035,#4035,#3550,.T.);
#4827=EDGE_CURVE('',#4036,#4036,#3551,.T.);
#4828=EDGE_CURVE('',#4036,#4037,#2540,.T.);
#4829=EDGE_CURVE('',#4037,#4037,#3552,.T.);
#4830=EDGE_CURVE('',#4038,#4038,#3553,.T.);
#4831=EDGE_CURVE('',#4038,#4039,#2541,.T.);
#4832=EDGE_CURVE('',#4039,#4039,#3554,.T.);
#4833=EDGE_CURVE('',#4040,#4040,#3555,.T.);
#4834=EDGE_CURVE('',#4040,#4041,#2542,.T.);
#4835=EDGE_CURVE('',#4041,#4041,#3556,.T.);
#4836=EDGE_CURVE('',#4042,#4042,#3557,.T.);
#4837=EDGE_CURVE('',#4042,#4043,#2543,.T.);
#4838=EDGE_CURVE('',#4043,#4043,#3558,.T.);
#4839=EDGE_CURVE('',#4044,#4044,#3559,.T.);
#4840=EDGE_CURVE('',#4044,#4045,#2544,.T.);
#4841=EDGE_CURVE('',#4045,#4045,#3560,.T.);
#4842=EDGE_CURVE('',#4046,#4046,#3561,.T.);
#4843=EDGE_CURVE('',#4046,#4047,#2545,.T.);
#4844=EDGE_CURVE('',#4047,#4047,#3562,.T.);
#4845=EDGE_CURVE('',#4048,#4048,#3563,.T.);
#4846=EDGE_CURVE('',#4048,#4049,#2546,.T.);
#4847=EDGE_CURVE('',#4049,#4049,#3564,.T.);
#4848=EDGE_CURVE('',#4050,#4051,#2547,.T.);
#4849=EDGE_CURVE('',#4050,#4052,#2548,.T.);
#4850=EDGE_CURVE('',#4053,#4052,#2549,.T.);
#4851=EDGE_CURVE('',#4051,#4053,#2550,.T.);
#4852=EDGE_CURVE('',#4054,#4055,#2551,.T.);
#4853=EDGE_CURVE('',#4056,#4054,#2552,.T.);
#4854=EDGE_CURVE('',#4057,#4056,#2553,.T.);
#4855=EDGE_CURVE('',#4055,#4057,#2554,.T.);
#4856=EDGE_CURVE('',#4055,#4050,#2555,.T.);
#4857=EDGE_CURVE('',#4052,#4057,#2556,.T.);
#4858=EDGE_CURVE('',#4053,#4056,#2557,.T.);
#4859=EDGE_CURVE('',#4054,#4051,#2558,.T.);
#4860=EDGE_CURVE('',#4058,#4058,#3565,.T.);
#4861=EDGE_CURVE('',#4058,#4059,#2559,.T.);
#4862=EDGE_CURVE('',#4059,#4059,#3566,.T.);
#4863=EDGE_CURVE('',#4060,#4060,#3567,.T.);
#4864=EDGE_CURVE('',#4060,#4061,#2560,.T.);
#4865=EDGE_CURVE('',#4061,#4061,#3568,.T.);
#4866=EDGE_CURVE('',#4062,#4062,#3569,.T.);
#4867=EDGE_CURVE('',#4062,#4063,#2561,.T.);
#4868=EDGE_CURVE('',#4063,#4063,#3570,.T.);
#4869=EDGE_CURVE('',#4064,#4064,#3571,.T.);
#4870=EDGE_CURVE('',#4064,#4065,#2562,.T.);
#4871=EDGE_CURVE('',#4065,#4065,#3572,.T.);
#4872=EDGE_CURVE('',#4066,#4066,#3573,.T.);
#4873=EDGE_CURVE('',#4066,#4067,#2563,.T.);
#4874=EDGE_CURVE('',#4067,#4067,#3574,.T.);
#4875=EDGE_CURVE('',#4068,#4069,#2564,.T.);
#4876=EDGE_CURVE('',#4068,#4070,#2565,.T.);
#4877=EDGE_CURVE('',#4071,#4070,#2566,.T.);
#4878=EDGE_CURVE('',#4069,#4071,#2567,.T.);
#4879=EDGE_CURVE('',#4072,#4073,#2568,.T.);
#4880=EDGE_CURVE('',#4074,#4072,#2569,.T.);
#4881=EDGE_CURVE('',#4075,#4074,#2570,.T.);
#4882=EDGE_CURVE('',#4073,#4075,#2571,.T.);
#4883=EDGE_CURVE('',#4073,#4068,#2572,.T.);
#4884=EDGE_CURVE('',#4070,#4075,#2573,.T.);
#4885=EDGE_CURVE('',#4071,#4074,#2574,.T.);
#4886=EDGE_CURVE('',#4072,#4069,#2575,.T.);
#4887=EDGE_CURVE('',#4076,#4077,#2576,.T.);
#4888=EDGE_CURVE('',#4077,#4078,#2577,.T.);
#4889=EDGE_CURVE('',#4079,#4078,#2578,.T.);
#4890=EDGE_CURVE('',#4076,#4079,#2579,.T.);
#4891=EDGE_CURVE('',#4080,#4076,#2580,.T.);
#4892=EDGE_CURVE('',#4081,#4079,#2581,.T.);
#4893=EDGE_CURVE('',#4080,#4081,#2582,.T.);
#4894=EDGE_CURVE('',#4082,#4080,#2583,.T.);
#4895=EDGE_CURVE('',#4083,#4081,#2584,.T.);
#4896=EDGE_CURVE('',#4082,#4083,#2585,.T.);
#4897=EDGE_CURVE('',#4077,#4082,#2586,.T.);
#4898=EDGE_CURVE('',#4078,#4083,#2587,.T.);
#4899=EDGE_CURVE('',#4084,#4084,#3575,.T.);
#4900=EDGE_CURVE('',#4084,#4085,#2588,.T.);
#4901=EDGE_CURVE('',#4085,#4085,#3576,.T.);
#4902=EDGE_CURVE('',#4086,#4086,#3577,.T.);
#4903=EDGE_CURVE('',#4086,#4087,#2589,.T.);
#4904=EDGE_CURVE('',#4087,#4087,#3578,.T.);
#4905=EDGE_CURVE('',#4088,#4088,#3579,.T.);
#4906=EDGE_CURVE('',#4088,#4089,#2590,.T.);
#4907=EDGE_CURVE('',#4089,#4089,#3580,.T.);
#4908=EDGE_CURVE('',#4090,#4090,#3581,.T.);
#4909=EDGE_CURVE('',#4090,#4091,#2591,.T.);
#4910=EDGE_CURVE('',#4091,#4091,#3582,.T.);
#4911=EDGE_CURVE('',#4092,#4092,#3583,.T.);
#4912=EDGE_CURVE('',#4092,#4093,#2592,.T.);
#4913=EDGE_CURVE('',#4093,#4093,#3584,.T.);
#4914=EDGE_CURVE('',#4094,#4094,#3585,.T.);
#4915=EDGE_CURVE('',#4094,#4095,#2593,.T.);
#4916=EDGE_CURVE('',#4095,#4095,#3586,.T.);
#4917=EDGE_CURVE('',#4096,#4096,#3587,.T.);
#4918=EDGE_CURVE('',#4096,#4097,#2594,.T.);
#4919=EDGE_CURVE('',#4097,#4097,#3588,.T.);
#4920=EDGE_CURVE('',#4098,#4098,#3589,.T.);
#4921=EDGE_CURVE('',#4098,#4099,#2595,.T.);
#4922=EDGE_CURVE('',#4099,#4099,#3590,.T.);
#4923=EDGE_CURVE('',#4100,#4100,#3591,.T.);
#4924=EDGE_CURVE('',#4100,#4101,#2596,.T.);
#4925=EDGE_CURVE('',#4101,#4101,#3592,.T.);
#4926=EDGE_CURVE('',#4102,#4102,#3593,.T.);
#4927=EDGE_CURVE('',#4102,#4103,#2597,.T.);
#4928=EDGE_CURVE('',#4103,#4103,#3594,.T.);
#4929=EDGE_CURVE('',#4104,#4104,#3595,.T.);
#4930=EDGE_CURVE('',#4104,#4105,#2598,.T.);
#4931=EDGE_CURVE('',#4105,#4105,#3596,.T.);
#4932=EDGE_CURVE('',#4106,#4106,#3597,.T.);
#4933=EDGE_CURVE('',#4106,#4107,#2599,.T.);
#4934=EDGE_CURVE('',#4107,#4107,#3598,.T.);
#4935=EDGE_CURVE('',#4108,#4108,#3599,.T.);
#4936=EDGE_CURVE('',#4108,#4109,#2600,.T.);
#4937=EDGE_CURVE('',#4109,#4109,#3600,.T.);
#4938=EDGE_CURVE('',#4110,#4110,#3601,.T.);
#4939=EDGE_CURVE('',#4110,#4111,#2601,.T.);
#4940=EDGE_CURVE('',#4111,#4111,#3602,.T.);
#4941=EDGE_CURVE('',#4112,#4112,#3603,.T.);
#4942=EDGE_CURVE('',#4112,#4113,#2602,.T.);
#4943=EDGE_CURVE('',#4113,#4113,#3604,.T.);
#4944=EDGE_CURVE('',#4114,#4114,#3605,.T.);
#4945=EDGE_CURVE('',#4114,#4115,#2603,.T.);
#4946=EDGE_CURVE('',#4115,#4115,#3606,.T.);
#4947=EDGE_CURVE('',#4116,#4116,#3607,.T.);
#4948=EDGE_CURVE('',#4116,#4117,#2604,.T.);
#4949=EDGE_CURVE('',#4117,#4117,#3608,.T.);
#4950=EDGE_CURVE('',#4118,#4118,#3609,.T.);
#4951=EDGE_CURVE('',#4118,#4119,#2605,.T.);
#4952=EDGE_CURVE('',#4119,#4119,#3610,.T.);
#4953=EDGE_CURVE('',#4120,#4120,#3611,.T.);
#4954=EDGE_CURVE('',#4120,#4121,#2606,.T.);
#4955=EDGE_CURVE('',#4121,#4121,#3612,.T.);
#4956=EDGE_CURVE('',#4122,#4122,#3613,.T.);
#4957=EDGE_CURVE('',#4122,#4123,#2607,.T.);
#4958=EDGE_CURVE('',#4123,#4123,#3614,.T.);
#4959=EDGE_CURVE('',#4124,#4124,#3615,.T.);
#4960=EDGE_CURVE('',#4124,#4125,#2608,.T.);
#4961=EDGE_CURVE('',#4125,#4125,#3616,.T.);
#4962=EDGE_CURVE('',#4126,#4126,#3617,.T.);
#4963=EDGE_CURVE('',#4126,#4127,#2609,.T.);
#4964=EDGE_CURVE('',#4127,#4127,#3618,.T.);
#4965=EDGE_CURVE('',#4128,#4128,#3619,.T.);
#4966=EDGE_CURVE('',#4128,#4129,#2610,.T.);
#4967=EDGE_CURVE('',#4129,#4129,#3620,.T.);
#4968=EDGE_CURVE('',#4130,#4130,#3621,.T.);
#4969=EDGE_CURVE('',#4130,#4131,#2611,.T.);
#4970=EDGE_CURVE('',#4131,#4131,#3622,.T.);
#4971=EDGE_CURVE('',#4132,#4133,#3623,.T.);
#4972=EDGE_CURVE('',#4134,#4132,#2612,.T.);
#4973=EDGE_CURVE('',#4135,#4134,#2613,.T.);
#4974=EDGE_CURVE('',#4133,#4135,#2614,.T.);
#4975=EDGE_CURVE('',#4133,#4136,#2615,.T.);
#4976=EDGE_CURVE('',#4137,#4135,#2616,.T.);
#4977=EDGE_CURVE('',#4137,#4136,#2617,.T.);
#4978=EDGE_CURVE('',#4136,#4138,#3624,.T.);
#4979=EDGE_CURVE('',#4139,#4137,#2618,.T.);
#4980=EDGE_CURVE('',#4138,#4139,#2619,.T.);
#4981=EDGE_CURVE('',#4138,#4132,#2620,.T.);
#4982=EDGE_CURVE('',#4139,#4134,#2621,.T.);
#4983=EDGE_CURVE('',#4140,#4140,#3625,.T.);
#4984=EDGE_CURVE('',#4141,#4141,#3626,.T.);
#4985=EDGE_CURVE('',#4142,#4142,#3627,.T.);
#4986=EDGE_CURVE('',#4142,#4140,#2622,.T.);
#4987=EDGE_CURVE('',#4143,#4143,#3628,.T.);
#4988=EDGE_CURVE('',#4144,#4144,#3629,.T.);
#4989=EDGE_CURVE('',#4144,#4143,#2623,.T.);
#4990=EDGE_CURVE('',#4145,#4145,#3630,.T.);
#4991=EDGE_CURVE('',#4146,#4146,#3631,.T.);
#4992=EDGE_CURVE('',#4146,#4145,#2624,.T.);
#4993=EDGE_CURVE('',#4147,#4147,#3632,.T.);
#4994=EDGE_CURVE('',#4148,#4148,#3633,.T.);
#4995=EDGE_CURVE('',#4148,#4147,#2625,.T.);
#4996=EDGE_CURVE('',#4149,#4149,#3634,.T.);
#4997=EDGE_CURVE('',#4150,#4150,#3635,.T.);
#4998=EDGE_CURVE('',#4150,#4149,#2626,.T.);
#4999=EDGE_CURVE('',#4151,#4151,#3636,.T.);
#5000=EDGE_CURVE('',#4151,#4141,#2627,.T.);
#5001=EDGE_CURVE('',#4152,#4153,#3637,.T.);
#5002=EDGE_CURVE('',#4154,#4152,#2628,.T.);
#5003=EDGE_CURVE('',#4155,#4154,#3638,.T.);
#5004=EDGE_CURVE('',#4153,#4155,#2629,.T.);
#5005=EDGE_CURVE('',#4153,#4156,#2630,.T.);
#5006=EDGE_CURVE('',#4157,#4155,#2631,.T.);
#5007=EDGE_CURVE('',#4157,#4156,#2632,.T.);
#5008=EDGE_CURVE('',#4156,#4158,#3639,.T.);
#5009=EDGE_CURVE('',#4159,#4157,#3640,.T.);
#5010=EDGE_CURVE('',#4158,#4159,#2633,.T.);
#5011=EDGE_CURVE('',#4158,#4152,#2634,.T.);
#5012=EDGE_CURVE('',#4154,#4159,#2635,.T.);
#5013=EDGE_CURVE('',#4160,#4160,#3641,.T.);
#5014=EDGE_CURVE('',#4161,#4161,#3642,.T.);
#5015=EDGE_CURVE('',#4162,#4162,#3643,.T.);
#5016=EDGE_CURVE('',#4162,#4160,#2636,.T.);
#5017=EDGE_CURVE('',#4163,#4163,#3644,.T.);
#5018=EDGE_CURVE('',#4163,#4161,#2637,.T.);
#5019=EDGE_CURVE('',#4164,#4165,#2638,.T.);
#5020=EDGE_CURVE('',#4165,#4166,#2639,.T.);
#5021=EDGE_CURVE('',#4166,#4167,#2640,.T.);
#5022=EDGE_CURVE('',#4164,#4167,#2641,.T.);
#5023=EDGE_CURVE('',#4165,#4168,#2642,.T.);
#5024=EDGE_CURVE('',#4168,#4169,#2643,.T.);
#5025=EDGE_CURVE('',#4169,#4166,#2644,.T.);
#5026=EDGE_CURVE('',#4168,#4170,#2645,.T.);
#5027=EDGE_CURVE('',#4170,#4171,#2646,.T.);
#5028=EDGE_CURVE('',#4171,#4169,#2647,.T.);
#5029=EDGE_CURVE('',#4170,#4172,#2648,.T.);
#5030=EDGE_CURVE('',#4172,#4173,#2649,.T.);
#5031=EDGE_CURVE('',#4173,#4171,#2650,.T.);
#5032=EDGE_CURVE('',#4172,#4174,#2651,.T.);
#5033=EDGE_CURVE('',#4174,#4175,#2652,.T.);
#5034=EDGE_CURVE('',#4175,#4173,#2653,.T.);
#5035=EDGE_CURVE('',#4174,#4164,#2654,.T.);
#5036=EDGE_CURVE('',#4167,#4175,#2655,.T.);
#5037=EDGE_CURVE('',#4176,#4176,#3645,.T.);
#5038=EDGE_CURVE('',#4177,#4177,#3646,.T.);
#5039=EDGE_CURVE('',#4178,#4178,#3647,.T.);
#5040=EDGE_CURVE('',#4178,#4177,#2656,.T.);
#5041=EDGE_CURVE('',#4179,#4179,#3648,.T.);
#5042=EDGE_CURVE('',#4179,#4178,#2657,.T.);
#5043=EDGE_CURVE('',#4180,#4180,#3649,.T.);
#5044=EDGE_CURVE('',#4180,#4179,#2658,.T.);
#5045=EDGE_CURVE('',#4181,#4181,#3650,.T.);
#5046=EDGE_CURVE('',#4182,#4182,#3651,.F.);
#5047=EDGE_CURVE('',#4182,#4181,#2659,.T.);
#5048=EDGE_CURVE('',#4176,#4182,#2660,.T.);
#5049=EDGE_CURVE('',#4183,#4184,#2661,.T.);
#5050=EDGE_CURVE('',#4184,#4185,#2662,.T.);
#5051=EDGE_CURVE('',#4185,#4186,#2663,.T.);
#5052=EDGE_CURVE('',#4183,#4186,#2664,.T.);
#5053=EDGE_CURVE('',#4184,#4187,#2665,.T.);
#5054=EDGE_CURVE('',#4187,#4188,#2666,.T.);
#5055=EDGE_CURVE('',#4188,#4185,#2667,.T.);
#5056=EDGE_CURVE('',#4187,#4189,#2668,.T.);
#5057=EDGE_CURVE('',#4189,#4190,#2669,.T.);
#5058=EDGE_CURVE('',#4190,#4188,#2670,.T.);
#5059=EDGE_CURVE('',#4189,#4191,#2671,.T.);
#5060=EDGE_CURVE('',#4191,#4192,#2672,.T.);
#5061=EDGE_CURVE('',#4192,#4190,#2673,.T.);
#5062=EDGE_CURVE('',#4191,#4193,#2674,.T.);
#5063=EDGE_CURVE('',#4193,#4194,#2675,.T.);
#5064=EDGE_CURVE('',#4194,#4192,#2676,.T.);
#5065=EDGE_CURVE('',#4193,#4183,#2677,.T.);
#5066=EDGE_CURVE('',#4186,#4194,#2678,.T.);
#5067=EDGE_CURVE('',#4195,#4195,#3652,.T.);
#5068=EDGE_CURVE('',#4196,#4196,#3653,.T.);
#5069=EDGE_CURVE('',#4195,#4197,#2679,.T.);
#5070=EDGE_CURVE('',#4197,#4197,#3654,.T.);
#5071=EDGE_CURVE('',#4198,#4198,#3655,.T.);
#5072=EDGE_CURVE('',#4199,#4199,#3656,.T.);
#5073=EDGE_CURVE('',#4199,#4198,#2680,.T.);
#5074=EDGE_CURVE('',#4200,#4200,#3657,.T.);
#5075=EDGE_CURVE('',#4200,#4199,#2681,.T.);
#5076=EDGE_CURVE('',#4201,#4201,#3658,.T.);
#5077=EDGE_CURVE('',#4201,#4200,#2682,.T.);
#5078=EDGE_CURVE('',#4202,#4202,#3659,.T.);
#5079=EDGE_CURVE('',#4203,#4203,#3660,.F.);
#5080=EDGE_CURVE('',#4203,#4202,#2683,.T.);
#5081=EDGE_CURVE('',#4204,#4204,#3661,.F.);
#5082=EDGE_CURVE('',#4204,#4203,#2684,.T.);
#5083=EDGE_CURVE('',#4196,#4204,#2685,.T.);
#5084=EDGE_CURVE('',#4205,#4205,#3662,.T.);
#5085=EDGE_CURVE('',#4205,#4206,#2686,.T.);
#5086=EDGE_CURVE('',#4206,#4206,#3663,.T.);
#5087=EDGE_CURVE('',#4207,#4207,#3664,.T.);
#5088=EDGE_CURVE('',#4208,#4208,#3665,.T.);
#5089=EDGE_CURVE('',#4208,#4209,#2687,.T.);
#5090=EDGE_CURVE('',#4209,#4209,#3666,.T.);
#5091=EDGE_CURVE('',#4210,#4210,#3667,.T.);
#5092=EDGE_CURVE('',#4211,#4211,#3668,.T.);
#5093=EDGE_CURVE('',#4211,#4212,#2688,.T.);
#5094=EDGE_CURVE('',#4212,#4212,#3669,.T.);
#5095=EDGE_CURVE('',#4207,#4213,#2689,.T.);
#5096=EDGE_CURVE('',#4213,#4213,#3670,.T.);
#5097=EDGE_CURVE('',#4214,#4214,#3671,.T.);
#5098=EDGE_CURVE('',#4214,#4210,#2690,.T.);
#5099=EDGE_CURVE('',#4215,#4215,#3672,.T.);
#5100=EDGE_CURVE('',#4215,#4215,#3673,.T.);
#5101=EDGE_CURVE('',#4216,#4216,#3674,.T.);
#5102=EDGE_CURVE('',#4216,#4217,#2691,.T.);
#5103=EDGE_CURVE('',#4217,#4217,#3675,.T.);
#5104=EDGE_CURVE('',#4218,#4218,#3676,.T.);
#5105=EDGE_CURVE('',#4218,#4219,#2692,.T.);
#5106=EDGE_CURVE('',#4219,#4219,#3677,.T.);
#5107=EDGE_CURVE('',#4220,#4220,#3678,.T.);
#5108=EDGE_CURVE('',#4221,#4221,#3679,.T.);
#5109=EDGE_CURVE('',#4221,#4220,#2693,.T.);
#5110=EDGE_CURVE('',#4222,#4222,#3680,.T.);
#5111=EDGE_CURVE('',#4222,#4221,#2694,.T.);
#5112=EDGE_CURVE('',#4223,#4223,#3681,.T.);
#5113=EDGE_CURVE('',#4223,#4222,#2695,.T.);
#5114=EDGE_CURVE('',#4224,#4224,#3682,.T.);
#5115=EDGE_CURVE('',#4225,#4225,#3683,.F.);
#5116=EDGE_CURVE('',#4225,#4224,#2696,.T.);
#5117=EDGE_CURVE('',#4226,#4226,#3684,.F.);
#5118=EDGE_CURVE('',#4226,#4225,#2697,.T.);
#5119=EDGE_CURVE('',#4227,#4227,#3685,.T.);
#5120=EDGE_CURVE('',#4227,#4226,#2698,.T.);
#5121=EDGE_CURVE('',#4228,#4229,#2699,.T.);
#5122=EDGE_CURVE('',#4229,#4230,#2700,.T.);
#5123=EDGE_CURVE('',#4230,#4231,#2701,.T.);
#5124=EDGE_CURVE('',#4228,#4231,#2702,.T.);
#5125=EDGE_CURVE('',#4229,#4232,#2703,.T.);
#5126=EDGE_CURVE('',#4232,#4233,#2704,.T.);
#5127=EDGE_CURVE('',#4233,#4230,#2705,.T.);
#5128=EDGE_CURVE('',#4232,#4234,#2706,.T.);
#5129=EDGE_CURVE('',#4234,#4235,#2707,.T.);
#5130=EDGE_CURVE('',#4235,#4233,#2708,.T.);
#5131=EDGE_CURVE('',#4234,#4236,#2709,.T.);
#5132=EDGE_CURVE('',#4236,#4237,#2710,.T.);
#5133=EDGE_CURVE('',#4237,#4235,#2711,.T.);
#5134=EDGE_CURVE('',#4236,#4238,#2712,.T.);
#5135=EDGE_CURVE('',#4238,#4239,#2713,.T.);
#5136=EDGE_CURVE('',#4239,#4237,#2714,.T.);
#5137=EDGE_CURVE('',#4238,#4228,#2715,.T.);
#5138=EDGE_CURVE('',#4231,#4239,#2716,.T.);
#5139=EDGE_CURVE('',#4240,#4240,#3686,.T.);
#5140=EDGE_CURVE('',#4240,#4241,#2717,.T.);
#5141=EDGE_CURVE('',#4241,#4241,#3687,.T.);
#5142=EDGE_CURVE('',#4242,#4242,#3688,.T.);
#5143=EDGE_CURVE('',#4242,#4243,#2718,.T.);
#5144=EDGE_CURVE('',#4243,#4243,#3689,.T.);
#5145=EDGE_CURVE('',#4244,#4245,#2719,.T.);
#5146=EDGE_CURVE('',#4244,#4245,#3690,.T.);
#5147=EDGE_CURVE('',#4246,#4244,#11,.T.);
#5148=EDGE_CURVE('',#4247,#4246,#3691,.T.);
#5149=EDGE_CURVE('',#4247,#4248,#2720,.T.);
#5150=EDGE_CURVE('',#4248,#4248,#3692,.T.);
#5151=EDGE_CURVE('',#4249,#4247,#3693,.T.);
#5152=EDGE_CURVE('',#4245,#4249,#12,.T.);
#5153=EDGE_CURVE('',#4249,#4246,#2721,.T.);
#5154=EDGE_CURVE('',#4250,#4250,#3694,.T.);
#5155=EDGE_CURVE('',#4250,#4251,#2722,.T.);
#5156=EDGE_CURVE('',#4251,#4251,#3695,.T.);
#5157=EDGE_CURVE('',#4252,#4253,#2723,.T.);
#5158=EDGE_CURVE('',#4254,#4252,#2724,.T.);
#5159=EDGE_CURVE('',#4255,#4254,#2725,.T.);
#5160=EDGE_CURVE('',#4253,#4255,#2726,.T.);
#5161=EDGE_CURVE('',#4256,#4252,#2727,.T.);
#5162=EDGE_CURVE('',#4257,#4256,#2728,.T.);
#5163=EDGE_CURVE('',#4254,#4257,#2729,.T.);
#5164=EDGE_CURVE('',#4258,#4256,#2730,.T.);
#5165=EDGE_CURVE('',#4259,#4258,#2731,.T.);
#5166=EDGE_CURVE('',#4257,#4259,#2732,.T.);
#5167=EDGE_CURVE('',#4260,#4259,#2733,.T.);
#5168=EDGE_CURVE('',#4261,#4260,#2734,.T.);
#5169=EDGE_CURVE('',#4262,#4261,#2735,.T.);
#5170=EDGE_CURVE('',#4263,#4262,#2736,.T.);
#5171=EDGE_CURVE('',#4255,#4263,#2737,.T.);
#5172=EDGE_CURVE('',#4264,#4258,#2738,.T.);
#5173=EDGE_CURVE('',#4260,#4264,#2739,.T.);
#5174=EDGE_CURVE('',#4263,#4265,#2740,.T.);
#5175=EDGE_CURVE('',#4253,#4265,#2741,.T.);
#5176=EDGE_CURVE('',#4261,#4266,#2742,.T.);
#5177=EDGE_CURVE('',#4267,#4266,#2743,.T.);
#5178=EDGE_CURVE('',#4262,#4267,#2744,.T.);
#5179=EDGE_CURVE('',#4265,#4267,#2745,.T.);
#5180=EDGE_CURVE('',#4266,#4264,#2746,.T.);
#5181=EDGE_CURVE('',#4268,#4269,#2747,.T.);
#5182=EDGE_CURVE('',#4268,#4270,#2748,.T.);
#5183=EDGE_CURVE('',#4270,#4271,#2749,.T.);
#5184=EDGE_CURVE('',#4269,#4271,#2750,.T.);
#5185=EDGE_CURVE('',#4272,#4268,#2751,.T.);
#5186=EDGE_CURVE('',#4272,#4273,#2752,.T.);
#5187=EDGE_CURVE('',#4273,#4270,#2753,.T.);
#5188=EDGE_CURVE('',#4274,#4272,#2754,.T.);
#5189=EDGE_CURVE('',#4274,#4275,#2755,.T.);
#5190=EDGE_CURVE('',#4275,#4273,#2756,.T.);
#5191=EDGE_CURVE('',#4276,#4274,#2757,.T.);
#5192=EDGE_CURVE('',#4276,#4277,#2758,.T.);
#5193=EDGE_CURVE('',#4277,#4275,#2759,.T.);
#5194=EDGE_CURVE('',#4278,#4276,#2760,.T.);
#5195=EDGE_CURVE('',#4278,#4279,#2761,.T.);
#5196=EDGE_CURVE('',#4279,#4277,#2762,.T.);
#5197=EDGE_CURVE('',#4269,#4278,#2763,.T.);
#5198=EDGE_CURVE('',#4271,#4279,#2764,.T.);
#5199=EDGE_CURVE('',#4280,#4280,#3696,.T.);
#5200=EDGE_CURVE('',#4281,#4281,#3697,.T.);
#5201=EDGE_CURVE('',#4281,#4280,#2765,.T.);
#5202=EDGE_CURVE('',#4282,#4282,#3698,.F.);
#5203=EDGE_CURVE('',#4282,#4281,#2766,.T.);
#5204=EDGE_CURVE('',#4283,#4283,#3699,.T.);
#5205=EDGE_CURVE('',#4283,#4282,#2767,.T.);
#5206=EDGE_CURVE('',#4284,#4285,#13,.T.);
#5207=EDGE_CURVE('',#4284,#4286,#2768,.T.);
#5208=EDGE_CURVE('',#4286,#4286,#14,.T.);
#5209=EDGE_CURVE('',#4287,#4284,#15,.T.);
#5210=EDGE_CURVE('',#4285,#4287,#16,.T.);
#5211=EDGE_CURVE('',#4288,#4288,#3700,.T.);
#5212=EDGE_CURVE('',#4289,#4289,#3701,.T.);
#5213=EDGE_CURVE('',#4289,#4288,#2769,.T.);
#5214=EDGE_CURVE('',#4290,#4290,#3702,.T.);
#5215=EDGE_CURVE('',#4290,#4289,#2770,.T.);
#5216=EDGE_CURVE('',#4291,#4291,#3703,.T.);
#5217=EDGE_CURVE('',#4292,#4292,#3704,.T.);
#5218=EDGE_CURVE('',#4292,#4285,#2771,.T.);
#5219=EDGE_CURVE('',#4287,#4291,#2772,.T.);
#5220=EDGE_CURVE('',#4293,#4293,#3705,.T.);
#5221=EDGE_CURVE('',#4293,#4292,#2773,.T.);
#5222=EDGE_CURVE('',#4294,#4294,#3706,.T.);
#5223=EDGE_CURVE('',#4294,#4295,#2774,.T.);
#5224=EDGE_CURVE('',#4295,#4295,#3707,.T.);
#5225=EDGE_CURVE('',#4296,#4296,#3708,.T.);
#5226=EDGE_CURVE('',#4296,#4297,#2775,.T.);
#5227=EDGE_CURVE('',#4297,#4297,#3709,.T.);
#5228=EDGE_CURVE('',#4298,#4298,#3710,.T.);
#5229=EDGE_CURVE('',#4298,#4298,#3711,.T.);
#5230=EDGE_CURVE('',#4299,#4300,#17,.T.);
#5231=EDGE_CURVE('',#4300,#4299,#18,.T.);
#5232=EDGE_CURVE('',#4301,#4302,#3712,.T.);
#5233=EDGE_CURVE('',#4301,#4302,#2776,.T.);
#5234=EDGE_CURVE('',#4302,#4303,#2777,.T.);
#5235=EDGE_CURVE('',#4304,#4303,#2778,.T.);
#5236=EDGE_CURVE('',#4301,#4304,#2779,.T.);
#5237=EDGE_CURVE('',#4305,#4304,#3713,.T.);
#5238=EDGE_CURVE('',#4305,#4300,#2780,.T.);
#5239=EDGE_CURVE('',#4303,#4305,#3714,.T.);
#5240=EDGE_CURVE('',#4306,#4306,#3715,.T.);
#5241=EDGE_CURVE('',#4306,#4307,#2781,.T.);
#5242=EDGE_CURVE('',#4307,#4307,#3716,.T.);
#5243=EDGE_CURVE('',#4308,#4308,#3717,.T.);
#5244=EDGE_CURVE('',#4308,#4309,#2782,.T.);
#5245=EDGE_CURVE('',#4309,#4309,#3718,.T.);
#5246=EDGE_CURVE('',#4310,#4310,#3719,.T.);
#5247=EDGE_CURVE('',#4310,#4311,#2783,.T.);
#5248=EDGE_CURVE('',#4311,#4311,#3720,.T.);
#5249=EDGE_CURVE('',#4312,#4312,#3721,.T.);
#5250=EDGE_CURVE('',#4312,#4313,#2784,.T.);
#5251=EDGE_CURVE('',#4313,#4313,#3722,.T.);
#5252=EDGE_CURVE('',#4314,#4314,#3723,.T.);
#5253=EDGE_CURVE('',#4314,#4315,#2785,.T.);
#5254=EDGE_CURVE('',#4315,#4315,#3724,.T.);
#5255=EDGE_CURVE('',#4316,#4316,#3725,.T.);
#5256=EDGE_CURVE('',#4316,#4317,#2786,.T.);
#5257=EDGE_CURVE('',#4317,#4317,#3726,.T.);
#5258=EDGE_CURVE('',#4318,#4318,#3727,.T.);
#5259=EDGE_CURVE('',#4318,#4319,#2787,.T.);
#5260=EDGE_CURVE('',#4319,#4319,#3728,.T.);
#5261=EDGE_CURVE('',#4320,#4321,#2788,.T.);
#5262=EDGE_CURVE('',#4322,#4320,#2789,.T.);
#5263=EDGE_CURVE('',#4323,#4322,#2790,.T.);
#5264=EDGE_CURVE('',#4321,#4323,#2791,.T.);
#5265=EDGE_CURVE('',#4324,#4320,#2792,.T.);
#5266=EDGE_CURVE('',#4325,#4324,#2793,.T.);
#5267=EDGE_CURVE('',#4322,#4325,#2794,.T.);
#5268=EDGE_CURVE('',#4326,#4325,#2795,.T.);
#5269=EDGE_CURVE('',#4323,#4326,#2796,.T.);
#5270=EDGE_CURVE('',#4321,#4327,#2797,.T.);
#5271=EDGE_CURVE('',#4327,#4326,#2798,.T.);
#5272=EDGE_CURVE('',#4327,#4324,#2799,.T.);
#5273=EDGE_CURVE('',#4328,#4329,#2800,.T.);
#5274=EDGE_CURVE('',#4329,#4330,#2801,.T.);
#5275=EDGE_CURVE('',#4331,#4330,#2802,.T.);
#5276=EDGE_CURVE('',#4328,#4331,#2803,.T.);
#5277=EDGE_CURVE('',#4332,#4328,#2804,.T.);
#5278=EDGE_CURVE('',#4333,#4331,#2805,.T.);
#5279=EDGE_CURVE('',#4332,#4333,#2806,.T.);
#5280=EDGE_CURVE('',#4334,#4332,#2807,.T.);
#5281=EDGE_CURVE('',#4335,#4333,#2808,.T.);
#5282=EDGE_CURVE('',#4334,#4335,#2809,.T.);
#5283=EDGE_CURVE('',#4329,#4334,#2810,.T.);
#5284=EDGE_CURVE('',#4330,#4335,#2811,.T.);
#5285=EDGE_CURVE('',#4336,#4336,#3729,.T.);
#5286=EDGE_CURVE('',#4336,#4337,#2812,.T.);
#5287=EDGE_CURVE('',#4337,#4337,#3730,.T.);
#5288=EDGE_CURVE('',#4338,#4338,#3731,.T.);
#5289=EDGE_CURVE('',#4338,#4339,#2813,.T.);
#5290=EDGE_CURVE('',#4339,#4339,#3732,.T.);
#5291=EDGE_CURVE('',#4340,#4341,#31,.T.);
#5292=EDGE_CURVE('',#4342,#4340,#32,.T.);
#5293=EDGE_CURVE('',#4342,#4343,#2814,.T.);
#5294=EDGE_CURVE('',#4343,#4343,#3733,.T.);
#5295=EDGE_CURVE('',#4344,#4342,#33,.T.);
#5296=EDGE_CURVE('',#4345,#4344,#34,.T.);
#5297=EDGE_CURVE('',#4346,#4345,#35,.T.);
#5298=EDGE_CURVE('',#4341,#4346,#36,.T.);
#5299=EDGE_CURVE('',#4347,#4347,#3734,.T.);
#5300=EDGE_CURVE('',#4347,#4348,#2815,.T.);
#5301=EDGE_CURVE('',#4349,#4348,#37,.T.);
#5302=EDGE_CURVE('',#4350,#4349,#38,.T.);
#5303=EDGE_CURVE('',#4351,#4350,#39,.T.);
#5304=EDGE_CURVE('',#4352,#4351,#40,.T.);
#5305=EDGE_CURVE('',#4353,#4352,#41,.T.);
#5306=EDGE_CURVE('',#4348,#4353,#42,.T.);
#5307=EDGE_CURVE('',#4344,#4353,#2816,.T.);
#5308=EDGE_CURVE('',#4345,#4352,#2817,.T.);
#5309=EDGE_CURVE('',#4342,#4348,#2818,.T.);
#5310=EDGE_CURVE('',#4340,#4349,#2819,.T.);
#5311=EDGE_CURVE('',#4354,#4354,#3735,.F.);
#5312=EDGE_CURVE('',#4354,#4355,#2820,.T.);
#5313=EDGE_CURVE('',#4355,#4355,#3736,.F.);
#5314=EDGE_CURVE('',#4341,#4350,#2821,.T.);
#5315=EDGE_CURVE('',#4346,#4351,#2822,.T.);
#5316=ORIENTED_EDGE('',*,*,#4356,.F.);
#5317=ORIENTED_EDGE('',*,*,#4357,.T.);
#5318=ORIENTED_EDGE('',*,*,#4358,.T.);
#5319=ORIENTED_EDGE('',*,*,#4357,.F.);
#5320=ORIENTED_EDGE('',*,*,#4358,.F.);
#5321=ORIENTED_EDGE('',*,*,#4359,.F.);
#5322=ORIENTED_EDGE('',*,*,#4360,.T.);
#5323=ORIENTED_EDGE('',*,*,#4361,.T.);
#5324=ORIENTED_EDGE('',*,*,#4360,.F.);
#5325=ORIENTED_EDGE('',*,*,#4361,.F.);
#5326=ORIENTED_EDGE('',*,*,#4362,.F.);
#5327=ORIENTED_EDGE('',*,*,#4363,.T.);
#5328=ORIENTED_EDGE('',*,*,#4364,.F.);
#5329=ORIENTED_EDGE('',*,*,#4365,.T.);
#5330=ORIENTED_EDGE('',*,*,#4366,.F.);
#5331=ORIENTED_EDGE('',*,*,#4367,.F.);
#5332=ORIENTED_EDGE('',*,*,#4365,.F.);
#5333=ORIENTED_EDGE('',*,*,#4368,.F.);
#5334=ORIENTED_EDGE('',*,*,#4363,.F.);
#5335=ORIENTED_EDGE('',*,*,#4369,.F.);
#5336=ORIENTED_EDGE('',*,*,#4370,.F.);
#5337=ORIENTED_EDGE('',*,*,#4371,.F.);
#5338=ORIENTED_EDGE('',*,*,#4372,.T.);
#5339=ORIENTED_EDGE('',*,*,#4373,.F.);
#5340=ORIENTED_EDGE('',*,*,#4374,.F.);
#5341=ORIENTED_EDGE('',*,*,#4375,.T.);
#5342=ORIENTED_EDGE('',*,*,#4376,.F.);
#5343=ORIENTED_EDGE('',*,*,#4377,.F.);
#5344=ORIENTED_EDGE('',*,*,#4372,.F.);
#5345=ORIENTED_EDGE('',*,*,#4378,.F.);
#5346=ORIENTED_EDGE('',*,*,#4379,.F.);
#5347=ORIENTED_EDGE('',*,*,#4380,.F.);
#5348=ORIENTED_EDGE('',*,*,#4381,.F.);
#5349=ORIENTED_EDGE('',*,*,#4382,.F.);
#5350=ORIENTED_EDGE('',*,*,#4375,.F.);
#5351=ORIENTED_EDGE('',*,*,#4383,.F.);
#5352=ORIENTED_EDGE('',*,*,#4380,.T.);
#5353=ORIENTED_EDGE('',*,*,#4369,.T.);
#5354=ORIENTED_EDGE('',*,*,#4384,.T.);
#5355=ORIENTED_EDGE('',*,*,#4362,.T.);
#5356=ORIENTED_EDGE('',*,*,#4385,.T.);
#5357=ORIENTED_EDGE('',*,*,#4370,.T.);
#5358=ORIENTED_EDGE('',*,*,#4384,.F.);
#5359=ORIENTED_EDGE('',*,*,#4367,.T.);
#5360=ORIENTED_EDGE('',*,*,#4383,.T.);
#5361=ORIENTED_EDGE('',*,*,#4379,.T.);
#5362=ORIENTED_EDGE('',*,*,#4386,.T.);
#5363=ORIENTED_EDGE('',*,*,#4387,.F.);
#5364=ORIENTED_EDGE('',*,*,#4386,.F.);
#5365=ORIENTED_EDGE('',*,*,#4371,.T.);
#5366=ORIENTED_EDGE('',*,*,#4366,.T.);
#5367=ORIENTED_EDGE('',*,*,#4364,.T.);
#5368=ORIENTED_EDGE('',*,*,#4385,.F.);
#5369=ORIENTED_EDGE('',*,*,#4378,.T.);
#5370=ORIENTED_EDGE('',*,*,#4381,.T.);
#5371=ORIENTED_EDGE('',*,*,#4388,.F.);
#5372=ORIENTED_EDGE('',*,*,#4376,.T.);
#5373=ORIENTED_EDGE('',*,*,#4382,.T.);
#5374=ORIENTED_EDGE('',*,*,#4374,.T.);
#5375=ORIENTED_EDGE('',*,*,#4389,.F.);
#5376=ORIENTED_EDGE('',*,*,#4390,.T.);
#5377=ORIENTED_EDGE('',*,*,#4391,.F.);
#5378=ORIENTED_EDGE('',*,*,#4390,.F.);
#5379=ORIENTED_EDGE('',*,*,#4392,.F.);
#5380=ORIENTED_EDGE('',*,*,#4368,.T.);
#5381=ORIENTED_EDGE('',*,*,#4388,.T.);
#5382=ORIENTED_EDGE('',*,*,#4393,.F.);
#5383=ORIENTED_EDGE('',*,*,#4394,.T.);
#5384=ORIENTED_EDGE('',*,*,#4395,.F.);
#5385=ORIENTED_EDGE('',*,*,#4394,.F.);
#5386=ORIENTED_EDGE('',*,*,#4393,.T.);
#5387=ORIENTED_EDGE('',*,*,#4387,.T.);
#5388=ORIENTED_EDGE('',*,*,#4396,.F.);
#5389=ORIENTED_EDGE('',*,*,#4397,.T.);
#5390=ORIENTED_EDGE('',*,*,#4398,.F.);
#5391=ORIENTED_EDGE('',*,*,#4397,.F.);
#5392=ORIENTED_EDGE('',*,*,#4399,.F.);
#5393=ORIENTED_EDGE('',*,*,#4400,.T.);
#5394=ORIENTED_EDGE('',*,*,#4401,.F.);
#5395=ORIENTED_EDGE('',*,*,#4400,.F.);
#5396=ORIENTED_EDGE('',*,*,#4402,.F.);
#5397=ORIENTED_EDGE('',*,*,#4403,.T.);
#5398=ORIENTED_EDGE('',*,*,#4404,.F.);
#5399=ORIENTED_EDGE('',*,*,#4403,.F.);
#5400=ORIENTED_EDGE('',*,*,#4405,.F.);
#5401=ORIENTED_EDGE('',*,*,#4406,.T.);
#5402=ORIENTED_EDGE('',*,*,#4407,.F.);
#5403=ORIENTED_EDGE('',*,*,#4406,.F.);
#5404=ORIENTED_EDGE('',*,*,#4408,.F.);
#5405=ORIENTED_EDGE('',*,*,#4409,.T.);
#5406=ORIENTED_EDGE('',*,*,#4410,.F.);
#5407=ORIENTED_EDGE('',*,*,#4409,.F.);
#5408=ORIENTED_EDGE('',*,*,#4373,.T.);
#5409=ORIENTED_EDGE('',*,*,#4377,.T.);
#5410=ORIENTED_EDGE('',*,*,#4392,.T.);
#5411=ORIENTED_EDGE('',*,*,#4389,.T.);
#5412=ORIENTED_EDGE('',*,*,#4410,.T.);
#5413=ORIENTED_EDGE('',*,*,#4411,.T.);
#5414=ORIENTED_EDGE('',*,*,#4412,.T.);
#5415=ORIENTED_EDGE('',*,*,#4413,.F.);
#5416=ORIENTED_EDGE('',*,*,#4414,.F.);
#5417=ORIENTED_EDGE('',*,*,#4391,.T.);
#5418=ORIENTED_EDGE('',*,*,#4407,.T.);
#5419=ORIENTED_EDGE('',*,*,#4404,.T.);
#5420=ORIENTED_EDGE('',*,*,#4401,.T.);
#5421=ORIENTED_EDGE('',*,*,#4398,.T.);
#5422=ORIENTED_EDGE('',*,*,#4415,.T.);
#5423=ORIENTED_EDGE('',*,*,#4414,.T.);
#5424=ORIENTED_EDGE('',*,*,#4416,.F.);
#5425=ORIENTED_EDGE('',*,*,#4417,.F.);
#5426=ORIENTED_EDGE('',*,*,#4418,.T.);
#5427=ORIENTED_EDGE('',*,*,#4417,.T.);
#5428=ORIENTED_EDGE('',*,*,#4419,.F.);
#5429=ORIENTED_EDGE('',*,*,#4420,.F.);
#5430=ORIENTED_EDGE('',*,*,#4408,.T.);
#5431=ORIENTED_EDGE('',*,*,#4405,.T.);
#5432=ORIENTED_EDGE('',*,*,#4402,.T.);
#5433=ORIENTED_EDGE('',*,*,#4399,.T.);
#5434=ORIENTED_EDGE('',*,*,#4396,.T.);
#5435=ORIENTED_EDGE('',*,*,#4421,.T.);
#5436=ORIENTED_EDGE('',*,*,#4420,.T.);
#5437=ORIENTED_EDGE('',*,*,#4422,.F.);
#5438=ORIENTED_EDGE('',*,*,#4412,.F.);
#5439=ORIENTED_EDGE('',*,*,#4422,.T.);
#5440=ORIENTED_EDGE('',*,*,#4419,.T.);
#5441=ORIENTED_EDGE('',*,*,#4416,.T.);
#5442=ORIENTED_EDGE('',*,*,#4413,.T.);
#5443=ORIENTED_EDGE('',*,*,#4395,.T.);
#5444=ORIENTED_EDGE('',*,*,#4421,.F.);
#5445=ORIENTED_EDGE('',*,*,#4411,.F.);
#5446=ORIENTED_EDGE('',*,*,#4415,.F.);
#5447=ORIENTED_EDGE('',*,*,#4418,.F.);
#5448=ORIENTED_EDGE('',*,*,#4356,.T.);
#5449=ORIENTED_EDGE('',*,*,#4359,.T.);
#5450=ORIENTED_EDGE('',*,*,#4423,.F.);
#5451=ORIENTED_EDGE('',*,*,#4424,.T.);
#5452=ORIENTED_EDGE('',*,*,#4425,.F.);
#5453=ORIENTED_EDGE('',*,*,#4424,.F.);
#5454=ORIENTED_EDGE('',*,*,#4423,.T.);
#5455=ORIENTED_EDGE('',*,*,#4426,.F.);
#5456=ORIENTED_EDGE('',*,*,#4427,.F.);
#5457=ORIENTED_EDGE('',*,*,#4428,.F.);
#5458=ORIENTED_EDGE('',*,*,#4429,.F.);
#5459=ORIENTED_EDGE('',*,*,#4427,.T.);
#5460=ORIENTED_EDGE('',*,*,#4430,.F.);
#5461=ORIENTED_EDGE('',*,*,#4431,.T.);
#5462=ORIENTED_EDGE('',*,*,#4428,.T.);
#5463=ORIENTED_EDGE('',*,*,#4430,.T.);
#5464=ORIENTED_EDGE('',*,*,#4426,.T.);
#5465=ORIENTED_EDGE('',*,*,#4432,.F.);
#5466=ORIENTED_EDGE('',*,*,#4433,.F.);
#5467=ORIENTED_EDGE('',*,*,#4434,.T.);
#5468=ORIENTED_EDGE('',*,*,#4435,.T.);
#5469=ORIENTED_EDGE('',*,*,#4434,.F.);
#5470=ORIENTED_EDGE('',*,*,#4435,.F.);
#5471=ORIENTED_EDGE('',*,*,#4436,.F.);
#5472=ORIENTED_EDGE('',*,*,#4433,.T.);
#5473=ORIENTED_EDGE('',*,*,#4437,.F.);
#5474=ORIENTED_EDGE('',*,*,#4431,.F.);
#5475=ORIENTED_EDGE('',*,*,#4438,.T.);
#5476=ORIENTED_EDGE('',*,*,#4437,.T.);
#5477=ORIENTED_EDGE('',*,*,#4438,.F.);
#5478=ORIENTED_EDGE('',*,*,#4436,.T.);
#5479=ORIENTED_EDGE('',*,*,#4439,.T.);
#5480=ORIENTED_EDGE('',*,*,#4440,.F.);
#5481=ORIENTED_EDGE('',*,*,#4439,.F.);
#5482=ORIENTED_EDGE('',*,*,#4429,.T.);
#5483=ORIENTED_EDGE('',*,*,#4432,.T.);
#5484=ORIENTED_EDGE('',*,*,#4441,.F.);
#5485=ORIENTED_EDGE('',*,*,#4442,.T.);
#5486=ORIENTED_EDGE('',*,*,#4443,.T.);
#5487=ORIENTED_EDGE('',*,*,#4444,.T.);
#5488=ORIENTED_EDGE('',*,*,#4445,.F.);
#5489=ORIENTED_EDGE('',*,*,#4446,.F.);
#5490=ORIENTED_EDGE('',*,*,#4447,.F.);
#5491=ORIENTED_EDGE('',*,*,#4448,.T.);
#5492=ORIENTED_EDGE('',*,*,#4449,.T.);
#5493=ORIENTED_EDGE('',*,*,#4450,.F.);
#5494=ORIENTED_EDGE('',*,*,#4451,.F.);
#5495=ORIENTED_EDGE('',*,*,#4445,.T.);
#5496=ORIENTED_EDGE('',*,*,#4452,.F.);
#5497=ORIENTED_EDGE('',*,*,#4453,.T.);
#5498=ORIENTED_EDGE('',*,*,#4451,.T.);
#5499=ORIENTED_EDGE('',*,*,#4454,.F.);
#5500=ORIENTED_EDGE('',*,*,#4455,.F.);
#5501=ORIENTED_EDGE('',*,*,#4425,.T.);
#5502=ORIENTED_EDGE('',*,*,#4446,.T.);
#5503=ORIENTED_EDGE('',*,*,#4455,.T.);
#5504=ORIENTED_EDGE('',*,*,#4456,.F.);
#5505=ORIENTED_EDGE('',*,*,#4457,.F.);
#5506=ORIENTED_EDGE('',*,*,#4458,.T.);
#5507=ORIENTED_EDGE('',*,*,#4459,.F.);
#5508=ORIENTED_EDGE('',*,*,#4447,.T.);
#5509=ORIENTED_EDGE('',*,*,#4457,.T.);
#5510=ORIENTED_EDGE('',*,*,#4460,.F.);
#5511=ORIENTED_EDGE('',*,*,#4449,.F.);
#5512=ORIENTED_EDGE('',*,*,#4460,.T.);
#5513=ORIENTED_EDGE('',*,*,#4456,.T.);
#5514=ORIENTED_EDGE('',*,*,#4454,.T.);
#5515=ORIENTED_EDGE('',*,*,#4450,.T.);
#5516=ORIENTED_EDGE('',*,*,#4440,.T.);
#5517=ORIENTED_EDGE('',*,*,#4461,.T.);
#5518=ORIENTED_EDGE('',*,*,#4458,.F.);
#5519=ORIENTED_EDGE('',*,*,#4448,.F.);
#5520=ORIENTED_EDGE('',*,*,#4453,.F.);
#5521=ORIENTED_EDGE('',*,*,#4462,.T.);
#5522=ORIENTED_EDGE('',*,*,#4463,.T.);
#5523=ORIENTED_EDGE('',*,*,#4452,.T.);
#5524=ORIENTED_EDGE('',*,*,#4464,.T.);
#5525=ORIENTED_EDGE('',*,*,#4465,.T.);
#5526=ORIENTED_EDGE('',*,*,#4466,.F.);
#5527=ORIENTED_EDGE('',*,*,#4467,.F.);
#5528=ORIENTED_EDGE('',*,*,#4468,.F.);
#5529=ORIENTED_EDGE('',*,*,#4469,.F.);
#5530=ORIENTED_EDGE('',*,*,#4470,.F.);
#5531=ORIENTED_EDGE('',*,*,#4471,.F.);
#5532=ORIENTED_EDGE('',*,*,#4472,.T.);
#5533=ORIENTED_EDGE('',*,*,#4467,.T.);
#5534=ORIENTED_EDGE('',*,*,#4473,.T.);
#5535=ORIENTED_EDGE('',*,*,#4443,.F.);
#5536=ORIENTED_EDGE('',*,*,#4474,.F.);
#5537=ORIENTED_EDGE('',*,*,#4468,.T.);
#5538=ORIENTED_EDGE('',*,*,#4474,.T.);
#5539=ORIENTED_EDGE('',*,*,#4442,.F.);
#5540=ORIENTED_EDGE('',*,*,#4475,.F.);
#5541=ORIENTED_EDGE('',*,*,#4476,.F.);
#5542=ORIENTED_EDGE('',*,*,#4469,.T.);
#5543=ORIENTED_EDGE('',*,*,#4476,.T.);
#5544=ORIENTED_EDGE('',*,*,#4477,.F.);
#5545=ORIENTED_EDGE('',*,*,#4461,.F.);
#5546=ORIENTED_EDGE('',*,*,#4478,.F.);
#5547=ORIENTED_EDGE('',*,*,#4470,.T.);
#5548=ORIENTED_EDGE('',*,*,#4478,.T.);
#5549=ORIENTED_EDGE('',*,*,#4463,.F.);
#5550=ORIENTED_EDGE('',*,*,#4479,.F.);
#5551=ORIENTED_EDGE('',*,*,#4471,.T.);
#5552=ORIENTED_EDGE('',*,*,#4479,.T.);
#5553=ORIENTED_EDGE('',*,*,#4462,.F.);
#5554=ORIENTED_EDGE('',*,*,#4465,.F.);
#5555=ORIENTED_EDGE('',*,*,#4480,.F.);
#5556=ORIENTED_EDGE('',*,*,#4466,.T.);
#5557=ORIENTED_EDGE('',*,*,#4480,.T.);
#5558=ORIENTED_EDGE('',*,*,#4464,.F.);
#5559=ORIENTED_EDGE('',*,*,#4444,.F.);
#5560=ORIENTED_EDGE('',*,*,#4473,.F.);
#5561=ORIENTED_EDGE('',*,*,#4459,.T.);
#5562=ORIENTED_EDGE('',*,*,#4477,.T.);
#5563=ORIENTED_EDGE('',*,*,#4475,.T.);
#5564=ORIENTED_EDGE('',*,*,#4441,.T.);
#5565=ORIENTED_EDGE('',*,*,#4481,.T.);
#5566=ORIENTED_EDGE('',*,*,#4482,.T.);
#5567=ORIENTED_EDGE('',*,*,#4481,.F.);
#5568=ORIENTED_EDGE('',*,*,#4472,.F.);
#5569=ORIENTED_EDGE('',*,*,#4483,.T.);
#5570=ORIENTED_EDGE('',*,*,#4484,.T.);
#5571=ORIENTED_EDGE('',*,*,#4483,.F.);
#5572=ORIENTED_EDGE('',*,*,#4484,.F.);
#5573=ORIENTED_EDGE('',*,*,#4482,.F.);
#5574=ORIENTED_EDGE('',*,*,#4485,.F.);
#5575=ORIENTED_EDGE('',*,*,#4486,.T.);
#5576=ORIENTED_EDGE('',*,*,#4486,.F.);
#5577=ORIENTED_EDGE('',*,*,#4487,.F.);
#5578=ORIENTED_EDGE('',*,*,#4488,.T.);
#5579=ORIENTED_EDGE('',*,*,#4485,.T.);
#5580=ORIENTED_EDGE('',*,*,#4488,.F.);
#5581=ORIENTED_EDGE('',*,*,#4489,.F.);
#5582=ORIENTED_EDGE('',*,*,#4490,.T.);
#5583=ORIENTED_EDGE('',*,*,#4487,.T.);
#5584=ORIENTED_EDGE('',*,*,#4490,.F.);
#5585=ORIENTED_EDGE('',*,*,#4491,.F.);
#5586=ORIENTED_EDGE('',*,*,#4489,.T.);
#5587=ORIENTED_EDGE('',*,*,#4492,.F.);
#5588=ORIENTED_EDGE('',*,*,#4493,.T.);
#5589=ORIENTED_EDGE('',*,*,#4491,.T.);
#5590=ORIENTED_EDGE('',*,*,#4493,.F.);
#5591=ORIENTED_EDGE('',*,*,#4492,.T.);
#5592=ORIENTED_EDGE('',*,*,#4494,.F.);
#5593=ORIENTED_EDGE('',*,*,#4495,.T.);
#5594=ORIENTED_EDGE('',*,*,#4496,.T.);
#5595=ORIENTED_EDGE('',*,*,#4495,.F.);
#5596=ORIENTED_EDGE('',*,*,#4496,.F.);
#5597=ORIENTED_EDGE('',*,*,#4497,.F.);
#5598=ORIENTED_EDGE('',*,*,#4498,.T.);
#5599=ORIENTED_EDGE('',*,*,#4499,.T.);
#5600=ORIENTED_EDGE('',*,*,#4498,.F.);
#5601=ORIENTED_EDGE('',*,*,#4499,.F.);
#5602=ORIENTED_EDGE('',*,*,#4500,.F.);
#5603=ORIENTED_EDGE('',*,*,#4501,.F.);
#5604=ORIENTED_EDGE('',*,*,#4502,.F.);
#5605=ORIENTED_EDGE('',*,*,#4503,.F.);
#5606=ORIENTED_EDGE('',*,*,#4504,.F.);
#5607=ORIENTED_EDGE('',*,*,#4505,.F.);
#5608=ORIENTED_EDGE('',*,*,#4506,.F.);
#5609=ORIENTED_EDGE('',*,*,#4507,.F.);
#5610=ORIENTED_EDGE('',*,*,#4508,.F.);
#5611=ORIENTED_EDGE('',*,*,#4509,.F.);
#5612=ORIENTED_EDGE('',*,*,#4510,.T.);
#5613=ORIENTED_EDGE('',*,*,#4511,.F.);
#5614=ORIENTED_EDGE('',*,*,#4512,.F.);
#5615=ORIENTED_EDGE('',*,*,#4513,.F.);
#5616=ORIENTED_EDGE('',*,*,#4501,.T.);
#5617=ORIENTED_EDGE('',*,*,#4514,.F.);
#5618=ORIENTED_EDGE('',*,*,#4515,.F.);
#5619=ORIENTED_EDGE('',*,*,#4510,.F.);
#5620=ORIENTED_EDGE('',*,*,#4516,.F.);
#5621=ORIENTED_EDGE('',*,*,#4517,.F.);
#5622=ORIENTED_EDGE('',*,*,#4503,.T.);
#5623=ORIENTED_EDGE('',*,*,#4518,.F.);
#5624=ORIENTED_EDGE('',*,*,#4519,.F.);
#5625=ORIENTED_EDGE('',*,*,#4520,.F.);
#5626=ORIENTED_EDGE('',*,*,#4505,.T.);
#5627=ORIENTED_EDGE('',*,*,#4521,.F.);
#5628=ORIENTED_EDGE('',*,*,#4507,.T.);
#5629=ORIENTED_EDGE('',*,*,#4500,.T.);
#5630=ORIENTED_EDGE('',*,*,#4522,.T.);
#5631=ORIENTED_EDGE('',*,*,#4513,.T.);
#5632=ORIENTED_EDGE('',*,*,#4523,.T.);
#5633=ORIENTED_EDGE('',*,*,#4514,.T.);
#5634=ORIENTED_EDGE('',*,*,#4524,.T.);
#5635=ORIENTED_EDGE('',*,*,#4518,.T.);
#5636=ORIENTED_EDGE('',*,*,#4523,.F.);
#5637=ORIENTED_EDGE('',*,*,#4512,.T.);
#5638=ORIENTED_EDGE('',*,*,#4515,.T.);
#5639=ORIENTED_EDGE('',*,*,#4524,.F.);
#5640=ORIENTED_EDGE('',*,*,#4520,.T.);
#5641=ORIENTED_EDGE('',*,*,#4504,.T.);
#5642=ORIENTED_EDGE('',*,*,#4522,.F.);
#5643=ORIENTED_EDGE('',*,*,#4502,.T.);
#5644=ORIENTED_EDGE('',*,*,#4517,.T.);
#5645=ORIENTED_EDGE('',*,*,#4511,.T.);
#5646=ORIENTED_EDGE('',*,*,#4525,.T.);
#5647=ORIENTED_EDGE('',*,*,#4526,.F.);
#5648=ORIENTED_EDGE('',*,*,#4525,.F.);
#5649=ORIENTED_EDGE('',*,*,#4519,.T.);
#5650=ORIENTED_EDGE('',*,*,#4516,.T.);
#5651=ORIENTED_EDGE('',*,*,#4509,.T.);
#5652=ORIENTED_EDGE('',*,*,#4527,.F.);
#5653=ORIENTED_EDGE('',*,*,#4528,.F.);
#5654=ORIENTED_EDGE('',*,*,#4529,.F.);
#5655=ORIENTED_EDGE('',*,*,#4530,.T.);
#5656=ORIENTED_EDGE('',*,*,#4531,.F.);
#5657=ORIENTED_EDGE('',*,*,#4530,.F.);
#5658=ORIENTED_EDGE('',*,*,#4529,.T.);
#5659=ORIENTED_EDGE('',*,*,#4526,.T.);
#5660=ORIENTED_EDGE('',*,*,#4532,.F.);
#5661=ORIENTED_EDGE('',*,*,#4533,.T.);
#5662=ORIENTED_EDGE('',*,*,#4534,.F.);
#5663=ORIENTED_EDGE('',*,*,#4533,.F.);
#5664=ORIENTED_EDGE('',*,*,#4535,.F.);
#5665=ORIENTED_EDGE('',*,*,#4536,.T.);
#5666=ORIENTED_EDGE('',*,*,#4537,.F.);
#5667=ORIENTED_EDGE('',*,*,#4536,.F.);
#5668=ORIENTED_EDGE('',*,*,#4538,.F.);
#5669=ORIENTED_EDGE('',*,*,#4539,.T.);
#5670=ORIENTED_EDGE('',*,*,#4540,.F.);
#5671=ORIENTED_EDGE('',*,*,#4539,.F.);
#5672=ORIENTED_EDGE('',*,*,#4541,.F.);
#5673=ORIENTED_EDGE('',*,*,#4542,.T.);
#5674=ORIENTED_EDGE('',*,*,#4543,.F.);
#5675=ORIENTED_EDGE('',*,*,#4542,.F.);
#5676=ORIENTED_EDGE('',*,*,#4544,.F.);
#5677=ORIENTED_EDGE('',*,*,#4545,.T.);
#5678=ORIENTED_EDGE('',*,*,#4527,.T.);
#5679=ORIENTED_EDGE('',*,*,#4508,.T.);
#5680=ORIENTED_EDGE('',*,*,#4521,.T.);
#5681=ORIENTED_EDGE('',*,*,#4506,.T.);
#5682=ORIENTED_EDGE('',*,*,#4528,.T.);
#5683=ORIENTED_EDGE('',*,*,#4545,.F.);
#5684=ORIENTED_EDGE('',*,*,#4546,.T.);
#5685=ORIENTED_EDGE('',*,*,#4547,.T.);
#5686=ORIENTED_EDGE('',*,*,#4548,.F.);
#5687=ORIENTED_EDGE('',*,*,#4549,.F.);
#5688=ORIENTED_EDGE('',*,*,#4534,.T.);
#5689=ORIENTED_EDGE('',*,*,#4537,.T.);
#5690=ORIENTED_EDGE('',*,*,#4540,.T.);
#5691=ORIENTED_EDGE('',*,*,#4543,.T.);
#5692=ORIENTED_EDGE('',*,*,#4550,.T.);
#5693=ORIENTED_EDGE('',*,*,#4549,.T.);
#5694=ORIENTED_EDGE('',*,*,#4551,.F.);
#5695=ORIENTED_EDGE('',*,*,#4552,.F.);
#5696=ORIENTED_EDGE('',*,*,#4553,.T.);
#5697=ORIENTED_EDGE('',*,*,#4552,.T.);
#5698=ORIENTED_EDGE('',*,*,#4554,.F.);
#5699=ORIENTED_EDGE('',*,*,#4555,.F.);
#5700=ORIENTED_EDGE('',*,*,#4544,.T.);
#5701=ORIENTED_EDGE('',*,*,#4541,.T.);
#5702=ORIENTED_EDGE('',*,*,#4538,.T.);
#5703=ORIENTED_EDGE('',*,*,#4535,.T.);
#5704=ORIENTED_EDGE('',*,*,#4532,.T.);
#5705=ORIENTED_EDGE('',*,*,#4556,.T.);
#5706=ORIENTED_EDGE('',*,*,#4555,.T.);
#5707=ORIENTED_EDGE('',*,*,#4557,.F.);
#5708=ORIENTED_EDGE('',*,*,#4547,.F.);
#5709=ORIENTED_EDGE('',*,*,#4557,.T.);
#5710=ORIENTED_EDGE('',*,*,#4554,.T.);
#5711=ORIENTED_EDGE('',*,*,#4551,.T.);
#5712=ORIENTED_EDGE('',*,*,#4548,.T.);
#5713=ORIENTED_EDGE('',*,*,#4531,.T.);
#5714=ORIENTED_EDGE('',*,*,#4556,.F.);
#5715=ORIENTED_EDGE('',*,*,#4546,.F.);
#5716=ORIENTED_EDGE('',*,*,#4550,.F.);
#5717=ORIENTED_EDGE('',*,*,#4553,.F.);
#5718=ORIENTED_EDGE('',*,*,#4494,.T.);
#5719=ORIENTED_EDGE('',*,*,#4497,.T.);
#5720=ORIENTED_EDGE('',*,*,#4558,.F.);
#5721=ORIENTED_EDGE('',*,*,#4559,.T.);
#5722=ORIENTED_EDGE('',*,*,#4560,.F.);
#5723=ORIENTED_EDGE('',*,*,#4559,.F.);
#5724=ORIENTED_EDGE('',*,*,#4558,.T.);
#5725=ORIENTED_EDGE('',*,*,#4561,.F.);
#5726=ORIENTED_EDGE('',*,*,#4562,.F.);
#5727=ORIENTED_EDGE('',*,*,#4563,.F.);
#5728=ORIENTED_EDGE('',*,*,#4564,.F.);
#5729=ORIENTED_EDGE('',*,*,#4562,.T.);
#5730=ORIENTED_EDGE('',*,*,#4565,.F.);
#5731=ORIENTED_EDGE('',*,*,#4566,.T.);
#5732=ORIENTED_EDGE('',*,*,#4563,.T.);
#5733=ORIENTED_EDGE('',*,*,#4565,.T.);
#5734=ORIENTED_EDGE('',*,*,#4561,.T.);
#5735=ORIENTED_EDGE('',*,*,#4567,.F.);
#5736=ORIENTED_EDGE('',*,*,#4568,.F.);
#5737=ORIENTED_EDGE('',*,*,#4569,.T.);
#5738=ORIENTED_EDGE('',*,*,#4570,.T.);
#5739=ORIENTED_EDGE('',*,*,#4569,.F.);
#5740=ORIENTED_EDGE('',*,*,#4570,.F.);
#5741=ORIENTED_EDGE('',*,*,#4571,.F.);
#5742=ORIENTED_EDGE('',*,*,#4568,.T.);
#5743=ORIENTED_EDGE('',*,*,#4572,.F.);
#5744=ORIENTED_EDGE('',*,*,#4566,.F.);
#5745=ORIENTED_EDGE('',*,*,#4573,.T.);
#5746=ORIENTED_EDGE('',*,*,#4572,.T.);
#5747=ORIENTED_EDGE('',*,*,#4573,.F.);
#5748=ORIENTED_EDGE('',*,*,#4571,.T.);
#5749=ORIENTED_EDGE('',*,*,#4574,.T.);
#5750=ORIENTED_EDGE('',*,*,#4575,.F.);
#5751=ORIENTED_EDGE('',*,*,#4574,.F.);
#5752=ORIENTED_EDGE('',*,*,#4564,.T.);
#5753=ORIENTED_EDGE('',*,*,#4567,.T.);
#5754=ORIENTED_EDGE('',*,*,#4576,.F.);
#5755=ORIENTED_EDGE('',*,*,#4577,.T.);
#5756=ORIENTED_EDGE('',*,*,#4578,.T.);
#5757=ORIENTED_EDGE('',*,*,#4579,.T.);
#5758=ORIENTED_EDGE('',*,*,#4580,.F.);
#5759=ORIENTED_EDGE('',*,*,#4581,.F.);
#5760=ORIENTED_EDGE('',*,*,#4582,.F.);
#5761=ORIENTED_EDGE('',*,*,#4583,.T.);
#5762=ORIENTED_EDGE('',*,*,#4584,.T.);
#5763=ORIENTED_EDGE('',*,*,#4585,.F.);
#5764=ORIENTED_EDGE('',*,*,#4586,.F.);
#5765=ORIENTED_EDGE('',*,*,#4580,.T.);
#5766=ORIENTED_EDGE('',*,*,#4587,.F.);
#5767=ORIENTED_EDGE('',*,*,#4588,.T.);
#5768=ORIENTED_EDGE('',*,*,#4586,.T.);
#5769=ORIENTED_EDGE('',*,*,#4589,.F.);
#5770=ORIENTED_EDGE('',*,*,#4590,.F.);
#5771=ORIENTED_EDGE('',*,*,#4560,.T.);
#5772=ORIENTED_EDGE('',*,*,#4581,.T.);
#5773=ORIENTED_EDGE('',*,*,#4590,.T.);
#5774=ORIENTED_EDGE('',*,*,#4591,.F.);
#5775=ORIENTED_EDGE('',*,*,#4592,.F.);
#5776=ORIENTED_EDGE('',*,*,#4593,.T.);
#5777=ORIENTED_EDGE('',*,*,#4594,.F.);
#5778=ORIENTED_EDGE('',*,*,#4582,.T.);
#5779=ORIENTED_EDGE('',*,*,#4592,.T.);
#5780=ORIENTED_EDGE('',*,*,#4595,.F.);
#5781=ORIENTED_EDGE('',*,*,#4584,.F.);
#5782=ORIENTED_EDGE('',*,*,#4595,.T.);
#5783=ORIENTED_EDGE('',*,*,#4591,.T.);
#5784=ORIENTED_EDGE('',*,*,#4589,.T.);
#5785=ORIENTED_EDGE('',*,*,#4585,.T.);
#5786=ORIENTED_EDGE('',*,*,#4575,.T.);
#5787=ORIENTED_EDGE('',*,*,#4596,.T.);
#5788=ORIENTED_EDGE('',*,*,#4593,.F.);
#5789=ORIENTED_EDGE('',*,*,#4583,.F.);
#5790=ORIENTED_EDGE('',*,*,#4588,.F.);
#5791=ORIENTED_EDGE('',*,*,#4597,.T.);
#5792=ORIENTED_EDGE('',*,*,#4598,.T.);
#5793=ORIENTED_EDGE('',*,*,#4587,.T.);
#5794=ORIENTED_EDGE('',*,*,#4599,.T.);
#5795=ORIENTED_EDGE('',*,*,#4600,.T.);
#5796=ORIENTED_EDGE('',*,*,#4601,.F.);
#5797=ORIENTED_EDGE('',*,*,#4602,.F.);
#5798=ORIENTED_EDGE('',*,*,#4603,.F.);
#5799=ORIENTED_EDGE('',*,*,#4604,.F.);
#5800=ORIENTED_EDGE('',*,*,#4605,.F.);
#5801=ORIENTED_EDGE('',*,*,#4606,.F.);
#5802=ORIENTED_EDGE('',*,*,#4607,.T.);
#5803=ORIENTED_EDGE('',*,*,#4602,.T.);
#5804=ORIENTED_EDGE('',*,*,#4608,.T.);
#5805=ORIENTED_EDGE('',*,*,#4578,.F.);
#5806=ORIENTED_EDGE('',*,*,#4609,.F.);
#5807=ORIENTED_EDGE('',*,*,#4603,.T.);
#5808=ORIENTED_EDGE('',*,*,#4609,.T.);
#5809=ORIENTED_EDGE('',*,*,#4577,.F.);
#5810=ORIENTED_EDGE('',*,*,#4610,.F.);
#5811=ORIENTED_EDGE('',*,*,#4611,.F.);
#5812=ORIENTED_EDGE('',*,*,#4604,.T.);
#5813=ORIENTED_EDGE('',*,*,#4611,.T.);
#5814=ORIENTED_EDGE('',*,*,#4612,.F.);
#5815=ORIENTED_EDGE('',*,*,#4596,.F.);
#5816=ORIENTED_EDGE('',*,*,#4613,.F.);
#5817=ORIENTED_EDGE('',*,*,#4605,.T.);
#5818=ORIENTED_EDGE('',*,*,#4613,.T.);
#5819=ORIENTED_EDGE('',*,*,#4598,.F.);
#5820=ORIENTED_EDGE('',*,*,#4614,.F.);
#5821=ORIENTED_EDGE('',*,*,#4606,.T.);
#5822=ORIENTED_EDGE('',*,*,#4614,.T.);
#5823=ORIENTED_EDGE('',*,*,#4597,.F.);
#5824=ORIENTED_EDGE('',*,*,#4600,.F.);
#5825=ORIENTED_EDGE('',*,*,#4615,.F.);
#5826=ORIENTED_EDGE('',*,*,#4601,.T.);
#5827=ORIENTED_EDGE('',*,*,#4615,.T.);
#5828=ORIENTED_EDGE('',*,*,#4599,.F.);
#5829=ORIENTED_EDGE('',*,*,#4579,.F.);
#5830=ORIENTED_EDGE('',*,*,#4608,.F.);
#5831=ORIENTED_EDGE('',*,*,#4594,.T.);
#5832=ORIENTED_EDGE('',*,*,#4612,.T.);
#5833=ORIENTED_EDGE('',*,*,#4610,.T.);
#5834=ORIENTED_EDGE('',*,*,#4576,.T.);
#5835=ORIENTED_EDGE('',*,*,#4616,.T.);
#5836=ORIENTED_EDGE('',*,*,#4617,.T.);
#5837=ORIENTED_EDGE('',*,*,#4616,.F.);
#5838=ORIENTED_EDGE('',*,*,#4607,.F.);
#5839=ORIENTED_EDGE('',*,*,#4618,.T.);
#5840=ORIENTED_EDGE('',*,*,#4619,.T.);
#5841=ORIENTED_EDGE('',*,*,#4618,.F.);
#5842=ORIENTED_EDGE('',*,*,#4619,.F.);
#5843=ORIENTED_EDGE('',*,*,#4617,.F.);
#5844=ORIENTED_EDGE('',*,*,#4620,.F.);
#5845=ORIENTED_EDGE('',*,*,#4621,.T.);
#5846=ORIENTED_EDGE('',*,*,#4621,.F.);
#5847=ORIENTED_EDGE('',*,*,#4622,.F.);
#5848=ORIENTED_EDGE('',*,*,#4623,.T.);
#5849=ORIENTED_EDGE('',*,*,#4620,.T.);
#5850=ORIENTED_EDGE('',*,*,#4623,.F.);
#5851=ORIENTED_EDGE('',*,*,#4624,.F.);
#5852=ORIENTED_EDGE('',*,*,#4625,.T.);
#5853=ORIENTED_EDGE('',*,*,#4622,.T.);
#5854=ORIENTED_EDGE('',*,*,#4625,.F.);
#5855=ORIENTED_EDGE('',*,*,#4626,.F.);
#5856=ORIENTED_EDGE('',*,*,#4624,.T.);
#5857=ORIENTED_EDGE('',*,*,#4627,.F.);
#5858=ORIENTED_EDGE('',*,*,#4628,.T.);
#5859=ORIENTED_EDGE('',*,*,#4626,.T.);
#5860=ORIENTED_EDGE('',*,*,#4628,.F.);
#5861=ORIENTED_EDGE('',*,*,#4627,.T.);
#5862=ORIENTED_EDGE('',*,*,#4629,.F.);
#5863=ORIENTED_EDGE('',*,*,#4630,.T.);
#5864=ORIENTED_EDGE('',*,*,#4631,.T.);
#5865=ORIENTED_EDGE('',*,*,#4630,.F.);
#5866=ORIENTED_EDGE('',*,*,#4632,.F.);
#5867=ORIENTED_EDGE('',*,*,#4633,.T.);
#5868=ORIENTED_EDGE('',*,*,#4634,.T.);
#5869=ORIENTED_EDGE('',*,*,#4633,.F.);
#5870=ORIENTED_EDGE('',*,*,#4632,.T.);
#5871=ORIENTED_EDGE('',*,*,#4629,.T.);
#5872=ORIENTED_EDGE('',*,*,#4634,.F.);
#5873=ORIENTED_EDGE('',*,*,#4631,.F.);
#5874=ORIENTED_EDGE('',*,*,#4635,.F.);
#5875=ORIENTED_EDGE('',*,*,#4636,.T.);
#5876=ORIENTED_EDGE('',*,*,#4637,.T.);
#5877=ORIENTED_EDGE('',*,*,#4636,.F.);
#5878=ORIENTED_EDGE('',*,*,#4638,.F.);
#5879=ORIENTED_EDGE('',*,*,#4639,.T.);
#5880=ORIENTED_EDGE('',*,*,#4640,.T.);
#5881=ORIENTED_EDGE('',*,*,#4639,.F.);
#5882=ORIENTED_EDGE('',*,*,#4638,.T.);
#5883=ORIENTED_EDGE('',*,*,#4635,.T.);
#5884=ORIENTED_EDGE('',*,*,#4640,.F.);
#5885=ORIENTED_EDGE('',*,*,#4637,.F.);
#5886=ORIENTED_EDGE('',*,*,#4641,.F.);
#5887=ORIENTED_EDGE('',*,*,#4642,.T.);
#5888=ORIENTED_EDGE('',*,*,#4643,.T.);
#5889=ORIENTED_EDGE('',*,*,#4642,.F.);
#5890=ORIENTED_EDGE('',*,*,#4644,.F.);
#5891=ORIENTED_EDGE('',*,*,#4645,.T.);
#5892=ORIENTED_EDGE('',*,*,#4646,.T.);
#5893=ORIENTED_EDGE('',*,*,#4645,.F.);
#5894=ORIENTED_EDGE('',*,*,#4644,.T.);
#5895=ORIENTED_EDGE('',*,*,#4641,.T.);
#5896=ORIENTED_EDGE('',*,*,#4646,.F.);
#5897=ORIENTED_EDGE('',*,*,#4643,.F.);
#5898=ORIENTED_EDGE('',*,*,#4647,.F.);
#5899=ORIENTED_EDGE('',*,*,#4648,.T.);
#5900=ORIENTED_EDGE('',*,*,#4649,.F.);
#5901=ORIENTED_EDGE('',*,*,#4648,.F.);
#5902=ORIENTED_EDGE('',*,*,#4647,.T.);
#5903=ORIENTED_EDGE('',*,*,#4650,.F.);
#5904=ORIENTED_EDGE('',*,*,#4651,.F.);
#5905=ORIENTED_EDGE('',*,*,#4652,.T.);
#5906=ORIENTED_EDGE('',*,*,#4653,.F.);
#5907=ORIENTED_EDGE('',*,*,#4652,.F.);
#5908=ORIENTED_EDGE('',*,*,#4651,.T.);
#5909=ORIENTED_EDGE('',*,*,#4654,.F.);
#5910=ORIENTED_EDGE('',*,*,#4655,.F.);
#5911=ORIENTED_EDGE('',*,*,#4656,.T.);
#5912=ORIENTED_EDGE('',*,*,#4650,.T.);
#5913=ORIENTED_EDGE('',*,*,#4656,.F.);
#5914=ORIENTED_EDGE('',*,*,#4657,.F.);
#5915=ORIENTED_EDGE('',*,*,#4658,.T.);
#5916=ORIENTED_EDGE('',*,*,#4654,.T.);
#5917=ORIENTED_EDGE('',*,*,#4658,.F.);
#5918=ORIENTED_EDGE('',*,*,#4659,.F.);
#5919=ORIENTED_EDGE('',*,*,#4660,.T.);
#5920=ORIENTED_EDGE('',*,*,#4661,.T.);
#5921=ORIENTED_EDGE('',*,*,#4660,.F.);
#5922=ORIENTED_EDGE('',*,*,#4661,.F.);
#5923=ORIENTED_EDGE('',*,*,#4662,.F.);
#5924=ORIENTED_EDGE('',*,*,#4663,.F.);
#5925=ORIENTED_EDGE('',*,*,#4664,.T.);
#5926=ORIENTED_EDGE('',*,*,#4665,.T.);
#5927=ORIENTED_EDGE('',*,*,#4664,.F.);
#5928=ORIENTED_EDGE('',*,*,#4665,.F.);
#5929=ORIENTED_EDGE('',*,*,#4666,.F.);
#5930=ORIENTED_EDGE('',*,*,#4662,.T.);
#5931=ORIENTED_EDGE('',*,*,#4667,.T.);
#5932=ORIENTED_EDGE('',*,*,#4668,.F.);
#5933=ORIENTED_EDGE('',*,*,#4667,.F.);
#5934=ORIENTED_EDGE('',*,*,#4666,.T.);
#5935=ORIENTED_EDGE('',*,*,#4669,.T.);
#5936=ORIENTED_EDGE('',*,*,#4670,.F.);
#5937=ORIENTED_EDGE('',*,*,#4669,.F.);
#5938=ORIENTED_EDGE('',*,*,#4671,.T.);
#5939=ORIENTED_EDGE('',*,*,#4672,.T.);
#5940=ORIENTED_EDGE('',*,*,#4673,.F.);
#5941=ORIENTED_EDGE('',*,*,#4674,.F.);
#5942=ORIENTED_EDGE('',*,*,#4675,.T.);
#5943=ORIENTED_EDGE('',*,*,#4674,.T.);
#5944=ORIENTED_EDGE('',*,*,#4676,.F.);
#5945=ORIENTED_EDGE('',*,*,#4677,.F.);
#5946=ORIENTED_EDGE('',*,*,#4678,.T.);
#5947=ORIENTED_EDGE('',*,*,#4677,.T.);
#5948=ORIENTED_EDGE('',*,*,#4679,.F.);
#5949=ORIENTED_EDGE('',*,*,#4680,.F.);
#5950=ORIENTED_EDGE('',*,*,#4681,.T.);
#5951=ORIENTED_EDGE('',*,*,#4680,.T.);
#5952=ORIENTED_EDGE('',*,*,#4682,.F.);
#5953=ORIENTED_EDGE('',*,*,#4672,.F.);
#5954=ORIENTED_EDGE('',*,*,#4682,.T.);
#5955=ORIENTED_EDGE('',*,*,#4679,.T.);
#5956=ORIENTED_EDGE('',*,*,#4676,.T.);
#5957=ORIENTED_EDGE('',*,*,#4673,.T.);
#5958=ORIENTED_EDGE('',*,*,#4649,.T.);
#5959=ORIENTED_EDGE('',*,*,#4653,.T.);
#5960=ORIENTED_EDGE('',*,*,#4668,.T.);
#5961=ORIENTED_EDGE('',*,*,#4670,.T.);
#5962=ORIENTED_EDGE('',*,*,#4681,.F.);
#5963=ORIENTED_EDGE('',*,*,#4671,.F.);
#5964=ORIENTED_EDGE('',*,*,#4675,.F.);
#5965=ORIENTED_EDGE('',*,*,#4678,.F.);
#5966=ORIENTED_EDGE('',*,*,#4655,.T.);
#5967=ORIENTED_EDGE('',*,*,#4657,.T.);
#5968=ORIENTED_EDGE('',*,*,#4659,.T.);
#5969=ORIENTED_EDGE('',*,*,#4663,.T.);
#5970=ORIENTED_EDGE('',*,*,#4683,.F.);
#5971=ORIENTED_EDGE('',*,*,#4684,.F.);
#5972=ORIENTED_EDGE('',*,*,#4685,.T.);
#5973=ORIENTED_EDGE('',*,*,#4683,.T.);
#5974=ORIENTED_EDGE('',*,*,#4685,.F.);
#5975=ORIENTED_EDGE('',*,*,#4686,.F.);
#5976=ORIENTED_EDGE('',*,*,#4687,.T.);
#5977=ORIENTED_EDGE('',*,*,#4684,.T.);
#5978=ORIENTED_EDGE('',*,*,#4687,.F.);
#5979=ORIENTED_EDGE('',*,*,#4688,.F.);
#5980=ORIENTED_EDGE('',*,*,#4689,.T.);
#5981=ORIENTED_EDGE('',*,*,#4686,.T.);
#5982=ORIENTED_EDGE('',*,*,#4689,.F.);
#5983=ORIENTED_EDGE('',*,*,#4688,.T.);
#5984=ORIENTED_EDGE('',*,*,#4690,.F.);
#5985=ORIENTED_EDGE('',*,*,#4691,.F.);
#5986=ORIENTED_EDGE('',*,*,#4692,.T.);
#5987=ORIENTED_EDGE('',*,*,#4690,.T.);
#5988=ORIENTED_EDGE('',*,*,#4692,.F.);
#5989=ORIENTED_EDGE('',*,*,#4693,.F.);
#5990=ORIENTED_EDGE('',*,*,#4694,.T.);
#5991=ORIENTED_EDGE('',*,*,#4691,.T.);
#5992=ORIENTED_EDGE('',*,*,#4694,.F.);
#5993=ORIENTED_EDGE('',*,*,#4695,.F.);
#5994=ORIENTED_EDGE('',*,*,#4696,.T.);
#5995=ORIENTED_EDGE('',*,*,#4693,.T.);
#5996=ORIENTED_EDGE('',*,*,#4696,.F.);
#5997=ORIENTED_EDGE('',*,*,#4695,.T.);
#5998=ORIENTED_EDGE('',*,*,#4697,.T.);
#5999=ORIENTED_EDGE('',*,*,#4698,.T.);
#6000=ORIENTED_EDGE('',*,*,#4699,.T.);
#6001=ORIENTED_EDGE('',*,*,#4700,.F.);
#6002=ORIENTED_EDGE('',*,*,#4701,.T.);
#6003=ORIENTED_EDGE('',*,*,#4702,.T.);
#6004=ORIENTED_EDGE('',*,*,#4703,.T.);
#6005=ORIENTED_EDGE('',*,*,#4698,.F.);
#6006=ORIENTED_EDGE('',*,*,#4704,.T.);
#6007=ORIENTED_EDGE('',*,*,#4705,.T.);
#6008=ORIENTED_EDGE('',*,*,#4706,.T.);
#6009=ORIENTED_EDGE('',*,*,#4702,.F.);
#6010=ORIENTED_EDGE('',*,*,#4707,.T.);
#6011=ORIENTED_EDGE('',*,*,#4708,.T.);
#6012=ORIENTED_EDGE('',*,*,#4709,.T.);
#6013=ORIENTED_EDGE('',*,*,#4705,.F.);
#6014=ORIENTED_EDGE('',*,*,#4710,.T.);
#6015=ORIENTED_EDGE('',*,*,#4711,.T.);
#6016=ORIENTED_EDGE('',*,*,#4712,.T.);
#6017=ORIENTED_EDGE('',*,*,#4708,.F.);
#6018=ORIENTED_EDGE('',*,*,#4713,.T.);
#6019=ORIENTED_EDGE('',*,*,#4700,.T.);
#6020=ORIENTED_EDGE('',*,*,#4714,.T.);
#6021=ORIENTED_EDGE('',*,*,#4711,.F.);
#6022=ORIENTED_EDGE('',*,*,#4713,.F.);
#6023=ORIENTED_EDGE('',*,*,#4710,.F.);
#6024=ORIENTED_EDGE('',*,*,#4707,.F.);
#6025=ORIENTED_EDGE('',*,*,#4704,.F.);
#6026=ORIENTED_EDGE('',*,*,#4701,.F.);
#6027=ORIENTED_EDGE('',*,*,#4697,.F.);
#6028=ORIENTED_EDGE('',*,*,#4714,.F.);
#6029=ORIENTED_EDGE('',*,*,#4699,.F.);
#6030=ORIENTED_EDGE('',*,*,#4703,.F.);
#6031=ORIENTED_EDGE('',*,*,#4706,.F.);
#6032=ORIENTED_EDGE('',*,*,#4709,.F.);
#6033=ORIENTED_EDGE('',*,*,#4712,.F.);
#6034=ORIENTED_EDGE('',*,*,#4715,.F.);
#6035=ORIENTED_EDGE('',*,*,#4716,.T.);
#6036=ORIENTED_EDGE('',*,*,#4717,.F.);
#6037=ORIENTED_EDGE('',*,*,#4716,.F.);
#6038=ORIENTED_EDGE('',*,*,#4715,.T.);
#6039=ORIENTED_EDGE('',*,*,#4718,.F.);
#6040=ORIENTED_EDGE('',*,*,#4719,.T.);
#6041=ORIENTED_EDGE('',*,*,#4720,.T.);
#6042=ORIENTED_EDGE('',*,*,#4721,.T.);
#6043=ORIENTED_EDGE('',*,*,#4722,.T.);
#6044=ORIENTED_EDGE('',*,*,#4723,.T.);
#6045=ORIENTED_EDGE('',*,*,#4724,.T.);
#6046=ORIENTED_EDGE('',*,*,#4725,.T.);
#6047=ORIENTED_EDGE('',*,*,#4726,.F.);
#6048=ORIENTED_EDGE('',*,*,#4727,.F.);
#6049=ORIENTED_EDGE('',*,*,#4728,.F.);
#6050=ORIENTED_EDGE('',*,*,#4729,.F.);
#6051=ORIENTED_EDGE('',*,*,#4730,.F.);
#6052=ORIENTED_EDGE('',*,*,#4731,.F.);
#6053=ORIENTED_EDGE('',*,*,#4732,.F.);
#6054=ORIENTED_EDGE('',*,*,#4727,.T.);
#6055=ORIENTED_EDGE('',*,*,#4733,.T.);
#6056=ORIENTED_EDGE('',*,*,#4724,.F.);
#6057=ORIENTED_EDGE('',*,*,#4734,.F.);
#6058=ORIENTED_EDGE('',*,*,#4728,.T.);
#6059=ORIENTED_EDGE('',*,*,#4734,.T.);
#6060=ORIENTED_EDGE('',*,*,#4723,.F.);
#6061=ORIENTED_EDGE('',*,*,#4735,.F.);
#6062=ORIENTED_EDGE('',*,*,#4729,.T.);
#6063=ORIENTED_EDGE('',*,*,#4735,.T.);
#6064=ORIENTED_EDGE('',*,*,#4722,.F.);
#6065=ORIENTED_EDGE('',*,*,#4736,.F.);
#6066=ORIENTED_EDGE('',*,*,#4730,.T.);
#6067=ORIENTED_EDGE('',*,*,#4736,.T.);
#6068=ORIENTED_EDGE('',*,*,#4721,.F.);
#6069=ORIENTED_EDGE('',*,*,#4737,.F.);
#6070=ORIENTED_EDGE('',*,*,#4731,.T.);
#6071=ORIENTED_EDGE('',*,*,#4737,.T.);
#6072=ORIENTED_EDGE('',*,*,#4720,.F.);
#6073=ORIENTED_EDGE('',*,*,#4738,.F.);
#6074=ORIENTED_EDGE('',*,*,#4726,.T.);
#6075=ORIENTED_EDGE('',*,*,#4738,.T.);
#6076=ORIENTED_EDGE('',*,*,#4719,.F.);
#6077=ORIENTED_EDGE('',*,*,#4733,.F.);
#6078=ORIENTED_EDGE('',*,*,#4739,.F.);
#6079=ORIENTED_EDGE('',*,*,#4717,.T.);
#6080=ORIENTED_EDGE('',*,*,#4739,.T.);
#6081=ORIENTED_EDGE('',*,*,#4740,.T.);
#6082=ORIENTED_EDGE('',*,*,#4741,.F.);
#6083=ORIENTED_EDGE('',*,*,#4740,.F.);
#6084=ORIENTED_EDGE('',*,*,#4742,.F.);
#6085=ORIENTED_EDGE('',*,*,#4741,.T.);
#6086=ORIENTED_EDGE('',*,*,#4725,.F.);
#6087=ORIENTED_EDGE('',*,*,#4743,.T.);
#6088=ORIENTED_EDGE('',*,*,#4742,.T.);
#6089=ORIENTED_EDGE('',*,*,#4743,.F.);
#6090=ORIENTED_EDGE('',*,*,#4744,.F.);
#6091=ORIENTED_EDGE('',*,*,#4745,.T.);
#6092=ORIENTED_EDGE('',*,*,#4732,.T.);
#6093=ORIENTED_EDGE('',*,*,#4745,.F.);
#6094=ORIENTED_EDGE('',*,*,#4744,.T.);
#6095=ORIENTED_EDGE('',*,*,#4746,.F.);
#6096=ORIENTED_EDGE('',*,*,#4746,.T.);
#6097=ORIENTED_EDGE('',*,*,#4747,.T.);
#6098=ORIENTED_EDGE('',*,*,#4718,.T.);
#6099=ORIENTED_EDGE('',*,*,#4747,.F.);
#6100=ORIENTED_EDGE('',*,*,#4748,.F.);
#6101=ORIENTED_EDGE('',*,*,#4749,.T.);
#6102=ORIENTED_EDGE('',*,*,#4750,.F.);
#6103=ORIENTED_EDGE('',*,*,#4751,.T.);
#6104=ORIENTED_EDGE('',*,*,#4748,.T.);
#6105=ORIENTED_EDGE('',*,*,#4751,.F.);
#6106=ORIENTED_EDGE('',*,*,#4750,.T.);
#6107=ORIENTED_EDGE('',*,*,#4752,.F.);
#6108=ORIENTED_EDGE('',*,*,#4753,.F.);
#6109=ORIENTED_EDGE('',*,*,#4754,.T.);
#6110=ORIENTED_EDGE('',*,*,#4752,.T.);
#6111=ORIENTED_EDGE('',*,*,#4754,.F.);
#6112=ORIENTED_EDGE('',*,*,#4753,.T.);
#6113=ORIENTED_EDGE('',*,*,#4755,.F.);
#6114=ORIENTED_EDGE('',*,*,#4755,.T.);
#6115=ORIENTED_EDGE('',*,*,#4756,.T.);
#6116=ORIENTED_EDGE('',*,*,#4749,.F.);
#6117=ORIENTED_EDGE('',*,*,#4756,.F.);
#6118=ORIENTED_EDGE('',*,*,#4757,.F.);
#6119=ORIENTED_EDGE('',*,*,#4758,.T.);
#6120=ORIENTED_EDGE('',*,*,#4757,.T.);
#6121=ORIENTED_EDGE('',*,*,#4758,.F.);
#6122=ORIENTED_EDGE('',*,*,#4759,.F.);
#6123=ORIENTED_EDGE('',*,*,#4760,.T.);
#6124=ORIENTED_EDGE('',*,*,#4761,.T.);
#6125=ORIENTED_EDGE('',*,*,#4760,.F.);
#6126=ORIENTED_EDGE('',*,*,#4761,.F.);
#6127=ORIENTED_EDGE('',*,*,#4762,.F.);
#6128=ORIENTED_EDGE('',*,*,#4759,.T.);
#6129=ORIENTED_EDGE('',*,*,#4763,.F.);
#6130=ORIENTED_EDGE('',*,*,#4763,.T.);
#6131=ORIENTED_EDGE('',*,*,#4764,.T.);
#6132=ORIENTED_EDGE('',*,*,#4765,.T.);
#6133=ORIENTED_EDGE('',*,*,#4764,.F.);
#6134=ORIENTED_EDGE('',*,*,#4766,.F.);
#6135=ORIENTED_EDGE('',*,*,#4767,.T.);
#6136=ORIENTED_EDGE('',*,*,#4762,.T.);
#6137=ORIENTED_EDGE('',*,*,#4767,.F.);
#6138=ORIENTED_EDGE('',*,*,#4768,.F.);
#6139=ORIENTED_EDGE('',*,*,#4769,.T.);
#6140=ORIENTED_EDGE('',*,*,#4770,.T.);
#6141=ORIENTED_EDGE('',*,*,#4769,.F.);
#6142=ORIENTED_EDGE('',*,*,#4768,.T.);
#6143=ORIENTED_EDGE('',*,*,#4766,.T.);
#6144=ORIENTED_EDGE('',*,*,#4770,.F.);
#6145=ORIENTED_EDGE('',*,*,#4765,.F.);
#6146=ORIENTED_EDGE('',*,*,#4771,.F.);
#6147=ORIENTED_EDGE('',*,*,#4772,.T.);
#6148=ORIENTED_EDGE('',*,*,#4771,.T.);
#6149=ORIENTED_EDGE('',*,*,#4772,.F.);
#6150=ORIENTED_EDGE('',*,*,#4773,.F.);
#6151=ORIENTED_EDGE('',*,*,#4774,.T.);
#6152=ORIENTED_EDGE('',*,*,#4775,.T.);
#6153=ORIENTED_EDGE('',*,*,#4774,.F.);
#6154=ORIENTED_EDGE('',*,*,#4773,.T.);
#6155=ORIENTED_EDGE('',*,*,#4775,.F.);
#6156=ORIENTED_EDGE('',*,*,#4776,.T.);
#6157=ORIENTED_EDGE('',*,*,#4777,.T.);
#6158=ORIENTED_EDGE('',*,*,#4778,.T.);
#6159=ORIENTED_EDGE('',*,*,#4777,.F.);
#6160=ORIENTED_EDGE('',*,*,#4778,.F.);
#6161=ORIENTED_EDGE('',*,*,#4779,.T.);
#6162=ORIENTED_EDGE('',*,*,#4780,.T.);
#6163=ORIENTED_EDGE('',*,*,#4779,.F.);
#6164=ORIENTED_EDGE('',*,*,#4781,.T.);
#6165=ORIENTED_EDGE('',*,*,#4776,.F.);
#6166=ORIENTED_EDGE('',*,*,#4781,.F.);
#6167=ORIENTED_EDGE('',*,*,#4782,.T.);
#6168=ORIENTED_EDGE('',*,*,#4783,.T.);
#6169=ORIENTED_EDGE('',*,*,#4782,.F.);
#6170=ORIENTED_EDGE('',*,*,#4783,.F.);
#6171=ORIENTED_EDGE('',*,*,#4780,.F.);
#6172=ORIENTED_EDGE('',*,*,#4784,.F.);
#6173=ORIENTED_EDGE('',*,*,#4785,.F.);
#6174=ORIENTED_EDGE('',*,*,#4786,.T.);
#6175=ORIENTED_EDGE('',*,*,#4787,.F.);
#6176=ORIENTED_EDGE('',*,*,#4786,.F.);
#6177=ORIENTED_EDGE('',*,*,#4788,.F.);
#6178=ORIENTED_EDGE('',*,*,#4789,.F.);
#6179=ORIENTED_EDGE('',*,*,#4790,.F.);
#6180=ORIENTED_EDGE('',*,*,#4791,.F.);
#6181=ORIENTED_EDGE('',*,*,#4792,.F.);
#6182=ORIENTED_EDGE('',*,*,#4793,.T.);
#6183=ORIENTED_EDGE('',*,*,#4794,.F.);
#6184=ORIENTED_EDGE('',*,*,#4795,.F.);
#6185=ORIENTED_EDGE('',*,*,#4796,.F.);
#6186=ORIENTED_EDGE('',*,*,#4797,.F.);
#6187=ORIENTED_EDGE('',*,*,#4798,.F.);
#6188=ORIENTED_EDGE('',*,*,#4799,.F.);
#6189=ORIENTED_EDGE('',*,*,#4793,.F.);
#6190=ORIENTED_EDGE('',*,*,#4789,.T.);
#6191=ORIENTED_EDGE('',*,*,#4800,.T.);
#6192=ORIENTED_EDGE('',*,*,#4798,.T.);
#6193=ORIENTED_EDGE('',*,*,#4801,.F.);
#6194=ORIENTED_EDGE('',*,*,#4788,.T.);
#6195=ORIENTED_EDGE('',*,*,#4802,.T.);
#6196=ORIENTED_EDGE('',*,*,#4799,.T.);
#6197=ORIENTED_EDGE('',*,*,#4800,.F.);
#6198=ORIENTED_EDGE('',*,*,#4785,.T.);
#6199=ORIENTED_EDGE('',*,*,#4803,.T.);
#6200=ORIENTED_EDGE('',*,*,#4794,.T.);
#6201=ORIENTED_EDGE('',*,*,#4802,.F.);
#6202=ORIENTED_EDGE('',*,*,#4804,.F.);
#6203=ORIENTED_EDGE('',*,*,#4805,.T.);
#6204=ORIENTED_EDGE('',*,*,#4806,.T.);
#6205=ORIENTED_EDGE('',*,*,#4805,.F.);
#6206=ORIENTED_EDGE('',*,*,#4784,.T.);
#6207=ORIENTED_EDGE('',*,*,#4807,.T.);
#6208=ORIENTED_EDGE('',*,*,#4795,.T.);
#6209=ORIENTED_EDGE('',*,*,#4803,.F.);
#6210=ORIENTED_EDGE('',*,*,#4790,.T.);
#6211=ORIENTED_EDGE('',*,*,#4801,.T.);
#6212=ORIENTED_EDGE('',*,*,#4797,.T.);
#6213=ORIENTED_EDGE('',*,*,#4808,.F.);
#6214=ORIENTED_EDGE('',*,*,#4791,.T.);
#6215=ORIENTED_EDGE('',*,*,#4808,.T.);
#6216=ORIENTED_EDGE('',*,*,#4796,.T.);
#6217=ORIENTED_EDGE('',*,*,#4807,.F.);
#6218=ORIENTED_EDGE('',*,*,#4792,.T.);
#6219=ORIENTED_EDGE('',*,*,#4804,.T.);
#6220=ORIENTED_EDGE('',*,*,#4787,.T.);
#6221=ORIENTED_EDGE('',*,*,#4806,.F.);
#6222=ORIENTED_EDGE('',*,*,#4809,.F.);
#6223=ORIENTED_EDGE('',*,*,#4810,.T.);
#6224=ORIENTED_EDGE('',*,*,#4811,.F.);
#6225=ORIENTED_EDGE('',*,*,#4810,.F.);
#6226=ORIENTED_EDGE('',*,*,#4812,.F.);
#6227=ORIENTED_EDGE('',*,*,#4813,.T.);
#6228=ORIENTED_EDGE('',*,*,#4814,.F.);
#6229=ORIENTED_EDGE('',*,*,#4813,.F.);
#6230=ORIENTED_EDGE('',*,*,#4815,.F.);
#6231=ORIENTED_EDGE('',*,*,#4816,.T.);
#6232=ORIENTED_EDGE('',*,*,#4817,.F.);
#6233=ORIENTED_EDGE('',*,*,#4816,.F.);
#6234=ORIENTED_EDGE('',*,*,#4818,.F.);
#6235=ORIENTED_EDGE('',*,*,#4819,.T.);
#6236=ORIENTED_EDGE('',*,*,#4820,.F.);
#6237=ORIENTED_EDGE('',*,*,#4819,.F.);
#6238=ORIENTED_EDGE('',*,*,#4821,.F.);
#6239=ORIENTED_EDGE('',*,*,#4822,.T.);
#6240=ORIENTED_EDGE('',*,*,#4823,.F.);
#6241=ORIENTED_EDGE('',*,*,#4822,.F.);
#6242=ORIENTED_EDGE('',*,*,#4824,.F.);
#6243=ORIENTED_EDGE('',*,*,#4825,.T.);
#6244=ORIENTED_EDGE('',*,*,#4826,.F.);
#6245=ORIENTED_EDGE('',*,*,#4825,.F.);
#6246=ORIENTED_EDGE('',*,*,#4827,.F.);
#6247=ORIENTED_EDGE('',*,*,#4828,.T.);
#6248=ORIENTED_EDGE('',*,*,#4829,.F.);
#6249=ORIENTED_EDGE('',*,*,#4828,.F.);
#6250=ORIENTED_EDGE('',*,*,#4830,.F.);
#6251=ORIENTED_EDGE('',*,*,#4831,.T.);
#6252=ORIENTED_EDGE('',*,*,#4832,.F.);
#6253=ORIENTED_EDGE('',*,*,#4831,.F.);
#6254=ORIENTED_EDGE('',*,*,#4833,.F.);
#6255=ORIENTED_EDGE('',*,*,#4834,.T.);
#6256=ORIENTED_EDGE('',*,*,#4835,.F.);
#6257=ORIENTED_EDGE('',*,*,#4834,.F.);
#6258=ORIENTED_EDGE('',*,*,#4836,.F.);
#6259=ORIENTED_EDGE('',*,*,#4837,.T.);
#6260=ORIENTED_EDGE('',*,*,#4838,.F.);
#6261=ORIENTED_EDGE('',*,*,#4837,.F.);
#6262=ORIENTED_EDGE('',*,*,#4839,.F.);
#6263=ORIENTED_EDGE('',*,*,#4840,.T.);
#6264=ORIENTED_EDGE('',*,*,#4841,.F.);
#6265=ORIENTED_EDGE('',*,*,#4840,.F.);
#6266=ORIENTED_EDGE('',*,*,#4842,.F.);
#6267=ORIENTED_EDGE('',*,*,#4843,.T.);
#6268=ORIENTED_EDGE('',*,*,#4844,.F.);
#6269=ORIENTED_EDGE('',*,*,#4843,.F.);
#6270=ORIENTED_EDGE('',*,*,#4845,.F.);
#6271=ORIENTED_EDGE('',*,*,#4846,.T.);
#6272=ORIENTED_EDGE('',*,*,#4847,.F.);
#6273=ORIENTED_EDGE('',*,*,#4846,.F.);
#6274=ORIENTED_EDGE('',*,*,#4848,.F.);
#6275=ORIENTED_EDGE('',*,*,#4849,.T.);
#6276=ORIENTED_EDGE('',*,*,#4850,.F.);
#6277=ORIENTED_EDGE('',*,*,#4851,.F.);
#6278=ORIENTED_EDGE('',*,*,#4852,.F.);
#6279=ORIENTED_EDGE('',*,*,#4853,.F.);
#6280=ORIENTED_EDGE('',*,*,#4854,.F.);
#6281=ORIENTED_EDGE('',*,*,#4855,.F.);
#6282=ORIENTED_EDGE('',*,*,#4856,.F.);
#6283=ORIENTED_EDGE('',*,*,#4855,.T.);
#6284=ORIENTED_EDGE('',*,*,#4857,.F.);
#6285=ORIENTED_EDGE('',*,*,#4849,.F.);
#6286=ORIENTED_EDGE('',*,*,#4857,.T.);
#6287=ORIENTED_EDGE('',*,*,#4854,.T.);
#6288=ORIENTED_EDGE('',*,*,#4858,.F.);
#6289=ORIENTED_EDGE('',*,*,#4850,.T.);
#6290=ORIENTED_EDGE('',*,*,#4847,.T.);
#6291=ORIENTED_EDGE('',*,*,#4844,.T.);
#6292=ORIENTED_EDGE('',*,*,#4841,.T.);
#6293=ORIENTED_EDGE('',*,*,#4838,.T.);
#6294=ORIENTED_EDGE('',*,*,#4835,.T.);
#6295=ORIENTED_EDGE('',*,*,#4856,.T.);
#6296=ORIENTED_EDGE('',*,*,#4848,.T.);
#6297=ORIENTED_EDGE('',*,*,#4859,.F.);
#6298=ORIENTED_EDGE('',*,*,#4852,.T.);
#6299=ORIENTED_EDGE('',*,*,#4845,.T.);
#6300=ORIENTED_EDGE('',*,*,#4842,.T.);
#6301=ORIENTED_EDGE('',*,*,#4839,.T.);
#6302=ORIENTED_EDGE('',*,*,#4836,.T.);
#6303=ORIENTED_EDGE('',*,*,#4833,.T.);
#6304=ORIENTED_EDGE('',*,*,#4860,.F.);
#6305=ORIENTED_EDGE('',*,*,#4861,.T.);
#6306=ORIENTED_EDGE('',*,*,#4862,.F.);
#6307=ORIENTED_EDGE('',*,*,#4861,.F.);
#6308=ORIENTED_EDGE('',*,*,#4863,.F.);
#6309=ORIENTED_EDGE('',*,*,#4864,.T.);
#6310=ORIENTED_EDGE('',*,*,#4865,.F.);
#6311=ORIENTED_EDGE('',*,*,#4864,.F.);
#6312=ORIENTED_EDGE('',*,*,#4866,.F.);
#6313=ORIENTED_EDGE('',*,*,#4867,.T.);
#6314=ORIENTED_EDGE('',*,*,#4868,.F.);
#6315=ORIENTED_EDGE('',*,*,#4867,.F.);
#6316=ORIENTED_EDGE('',*,*,#4869,.F.);
#6317=ORIENTED_EDGE('',*,*,#4870,.T.);
#6318=ORIENTED_EDGE('',*,*,#4871,.F.);
#6319=ORIENTED_EDGE('',*,*,#4870,.F.);
#6320=ORIENTED_EDGE('',*,*,#4872,.F.);
#6321=ORIENTED_EDGE('',*,*,#4873,.T.);
#6322=ORIENTED_EDGE('',*,*,#4874,.F.);
#6323=ORIENTED_EDGE('',*,*,#4873,.F.);
#6324=ORIENTED_EDGE('',*,*,#4875,.F.);
#6325=ORIENTED_EDGE('',*,*,#4876,.T.);
#6326=ORIENTED_EDGE('',*,*,#4877,.F.);
#6327=ORIENTED_EDGE('',*,*,#4878,.F.);
#6328=ORIENTED_EDGE('',*,*,#4879,.F.);
#6329=ORIENTED_EDGE('',*,*,#4880,.F.);
#6330=ORIENTED_EDGE('',*,*,#4881,.F.);
#6331=ORIENTED_EDGE('',*,*,#4882,.F.);
#6332=ORIENTED_EDGE('',*,*,#4883,.F.);
#6333=ORIENTED_EDGE('',*,*,#4882,.T.);
#6334=ORIENTED_EDGE('',*,*,#4884,.F.);
#6335=ORIENTED_EDGE('',*,*,#4876,.F.);
#6336=ORIENTED_EDGE('',*,*,#4884,.T.);
#6337=ORIENTED_EDGE('',*,*,#4881,.T.);
#6338=ORIENTED_EDGE('',*,*,#4885,.F.);
#6339=ORIENTED_EDGE('',*,*,#4877,.T.);
#6340=ORIENTED_EDGE('',*,*,#4874,.T.);
#6341=ORIENTED_EDGE('',*,*,#4871,.T.);
#6342=ORIENTED_EDGE('',*,*,#4868,.T.);
#6343=ORIENTED_EDGE('',*,*,#4865,.T.);
#6344=ORIENTED_EDGE('',*,*,#4862,.T.);
#6345=ORIENTED_EDGE('',*,*,#4883,.T.);
#6346=ORIENTED_EDGE('',*,*,#4875,.T.);
#6347=ORIENTED_EDGE('',*,*,#4886,.F.);
#6348=ORIENTED_EDGE('',*,*,#4879,.T.);
#6349=ORIENTED_EDGE('',*,*,#4872,.T.);
#6350=ORIENTED_EDGE('',*,*,#4869,.T.);
#6351=ORIENTED_EDGE('',*,*,#4866,.T.);
#6352=ORIENTED_EDGE('',*,*,#4863,.T.);
#6353=ORIENTED_EDGE('',*,*,#4860,.T.);
#6354=ORIENTED_EDGE('',*,*,#4887,.T.);
#6355=ORIENTED_EDGE('',*,*,#4888,.T.);
#6356=ORIENTED_EDGE('',*,*,#4889,.F.);
#6357=ORIENTED_EDGE('',*,*,#4890,.F.);
#6358=ORIENTED_EDGE('',*,*,#4891,.T.);
#6359=ORIENTED_EDGE('',*,*,#4890,.T.);
#6360=ORIENTED_EDGE('',*,*,#4892,.F.);
#6361=ORIENTED_EDGE('',*,*,#4893,.F.);
#6362=ORIENTED_EDGE('',*,*,#4894,.T.);
#6363=ORIENTED_EDGE('',*,*,#4893,.T.);
#6364=ORIENTED_EDGE('',*,*,#4895,.F.);
#6365=ORIENTED_EDGE('',*,*,#4896,.F.);
#6366=ORIENTED_EDGE('',*,*,#4897,.T.);
#6367=ORIENTED_EDGE('',*,*,#4896,.T.);
#6368=ORIENTED_EDGE('',*,*,#4898,.F.);
#6369=ORIENTED_EDGE('',*,*,#4888,.F.);
#6370=ORIENTED_EDGE('',*,*,#4898,.T.);
#6371=ORIENTED_EDGE('',*,*,#4895,.T.);
#6372=ORIENTED_EDGE('',*,*,#4892,.T.);
#6373=ORIENTED_EDGE('',*,*,#4889,.T.);
#6374=ORIENTED_EDGE('',*,*,#4880,.T.);
#6375=ORIENTED_EDGE('',*,*,#4886,.T.);
#6376=ORIENTED_EDGE('',*,*,#4878,.T.);
#6377=ORIENTED_EDGE('',*,*,#4885,.T.);
#6378=ORIENTED_EDGE('',*,*,#4853,.T.);
#6379=ORIENTED_EDGE('',*,*,#4859,.T.);
#6380=ORIENTED_EDGE('',*,*,#4851,.T.);
#6381=ORIENTED_EDGE('',*,*,#4858,.T.);
#6382=ORIENTED_EDGE('',*,*,#4832,.T.);
#6383=ORIENTED_EDGE('',*,*,#4829,.T.);
#6384=ORIENTED_EDGE('',*,*,#4826,.T.);
#6385=ORIENTED_EDGE('',*,*,#4823,.T.);
#6386=ORIENTED_EDGE('',*,*,#4820,.T.);
#6387=ORIENTED_EDGE('',*,*,#4817,.T.);
#6388=ORIENTED_EDGE('',*,*,#4814,.T.);
#6389=ORIENTED_EDGE('',*,*,#4811,.T.);
#6390=ORIENTED_EDGE('',*,*,#4897,.F.);
#6391=ORIENTED_EDGE('',*,*,#4887,.F.);
#6392=ORIENTED_EDGE('',*,*,#4891,.F.);
#6393=ORIENTED_EDGE('',*,*,#4894,.F.);
#6394=ORIENTED_EDGE('',*,*,#4830,.T.);
#6395=ORIENTED_EDGE('',*,*,#4827,.T.);
#6396=ORIENTED_EDGE('',*,*,#4824,.T.);
#6397=ORIENTED_EDGE('',*,*,#4821,.T.);
#6398=ORIENTED_EDGE('',*,*,#4818,.T.);
#6399=ORIENTED_EDGE('',*,*,#4815,.T.);
#6400=ORIENTED_EDGE('',*,*,#4812,.T.);
#6401=ORIENTED_EDGE('',*,*,#4809,.T.);
#6402=ORIENTED_EDGE('',*,*,#4899,.F.);
#6403=ORIENTED_EDGE('',*,*,#4900,.T.);
#6404=ORIENTED_EDGE('',*,*,#4901,.F.);
#6405=ORIENTED_EDGE('',*,*,#4900,.F.);
#6406=ORIENTED_EDGE('',*,*,#4902,.F.);
#6407=ORIENTED_EDGE('',*,*,#4903,.T.);
#6408=ORIENTED_EDGE('',*,*,#4904,.F.);
#6409=ORIENTED_EDGE('',*,*,#4903,.F.);
#6410=ORIENTED_EDGE('',*,*,#4905,.F.);
#6411=ORIENTED_EDGE('',*,*,#4906,.T.);
#6412=ORIENTED_EDGE('',*,*,#4907,.F.);
#6413=ORIENTED_EDGE('',*,*,#4906,.F.);
#6414=ORIENTED_EDGE('',*,*,#4908,.F.);
#6415=ORIENTED_EDGE('',*,*,#4909,.T.);
#6416=ORIENTED_EDGE('',*,*,#4910,.F.);
#6417=ORIENTED_EDGE('',*,*,#4909,.F.);
#6418=ORIENTED_EDGE('',*,*,#4911,.F.);
#6419=ORIENTED_EDGE('',*,*,#4912,.T.);
#6420=ORIENTED_EDGE('',*,*,#4913,.T.);
#6421=ORIENTED_EDGE('',*,*,#4912,.F.);
#6422=ORIENTED_EDGE('',*,*,#4914,.F.);
#6423=ORIENTED_EDGE('',*,*,#4915,.T.);
#6424=ORIENTED_EDGE('',*,*,#4916,.T.);
#6425=ORIENTED_EDGE('',*,*,#4915,.F.);
#6426=ORIENTED_EDGE('',*,*,#4914,.T.);
#6427=ORIENTED_EDGE('',*,*,#4911,.T.);
#6428=ORIENTED_EDGE('',*,*,#4910,.T.);
#6429=ORIENTED_EDGE('',*,*,#4907,.T.);
#6430=ORIENTED_EDGE('',*,*,#4904,.T.);
#6431=ORIENTED_EDGE('',*,*,#4901,.T.);
#6432=ORIENTED_EDGE('',*,*,#4916,.F.);
#6433=ORIENTED_EDGE('',*,*,#4913,.F.);
#6434=ORIENTED_EDGE('',*,*,#4908,.T.);
#6435=ORIENTED_EDGE('',*,*,#4905,.T.);
#6436=ORIENTED_EDGE('',*,*,#4902,.T.);
#6437=ORIENTED_EDGE('',*,*,#4899,.T.);
#6438=ORIENTED_EDGE('',*,*,#4917,.F.);
#6439=ORIENTED_EDGE('',*,*,#4918,.T.);
#6440=ORIENTED_EDGE('',*,*,#4919,.F.);
#6441=ORIENTED_EDGE('',*,*,#4918,.F.);
#6442=ORIENTED_EDGE('',*,*,#4920,.F.);
#6443=ORIENTED_EDGE('',*,*,#4921,.T.);
#6444=ORIENTED_EDGE('',*,*,#4922,.F.);
#6445=ORIENTED_EDGE('',*,*,#4921,.F.);
#6446=ORIENTED_EDGE('',*,*,#4923,.F.);
#6447=ORIENTED_EDGE('',*,*,#4924,.T.);
#6448=ORIENTED_EDGE('',*,*,#4925,.F.);
#6449=ORIENTED_EDGE('',*,*,#4924,.F.);
#6450=ORIENTED_EDGE('',*,*,#4926,.F.);
#6451=ORIENTED_EDGE('',*,*,#4927,.T.);
#6452=ORIENTED_EDGE('',*,*,#4928,.F.);
#6453=ORIENTED_EDGE('',*,*,#4927,.F.);
#6454=ORIENTED_EDGE('',*,*,#4929,.F.);
#6455=ORIENTED_EDGE('',*,*,#4930,.T.);
#6456=ORIENTED_EDGE('',*,*,#4931,.T.);
#6457=ORIENTED_EDGE('',*,*,#4930,.F.);
#6458=ORIENTED_EDGE('',*,*,#4932,.F.);
#6459=ORIENTED_EDGE('',*,*,#4933,.T.);
#6460=ORIENTED_EDGE('',*,*,#4934,.T.);
#6461=ORIENTED_EDGE('',*,*,#4933,.F.);
#6462=ORIENTED_EDGE('',*,*,#4932,.T.);
#6463=ORIENTED_EDGE('',*,*,#4929,.T.);
#6464=ORIENTED_EDGE('',*,*,#4928,.T.);
#6465=ORIENTED_EDGE('',*,*,#4925,.T.);
#6466=ORIENTED_EDGE('',*,*,#4922,.T.);
#6467=ORIENTED_EDGE('',*,*,#4919,.T.);
#6468=ORIENTED_EDGE('',*,*,#4934,.F.);
#6469=ORIENTED_EDGE('',*,*,#4931,.F.);
#6470=ORIENTED_EDGE('',*,*,#4926,.T.);
#6471=ORIENTED_EDGE('',*,*,#4923,.T.);
#6472=ORIENTED_EDGE('',*,*,#4920,.T.);
#6473=ORIENTED_EDGE('',*,*,#4917,.T.);
#6474=ORIENTED_EDGE('',*,*,#4935,.F.);
#6475=ORIENTED_EDGE('',*,*,#4936,.T.);
#6476=ORIENTED_EDGE('',*,*,#4937,.F.);
#6477=ORIENTED_EDGE('',*,*,#4936,.F.);
#6478=ORIENTED_EDGE('',*,*,#4938,.F.);
#6479=ORIENTED_EDGE('',*,*,#4939,.T.);
#6480=ORIENTED_EDGE('',*,*,#4940,.F.);
#6481=ORIENTED_EDGE('',*,*,#4939,.F.);
#6482=ORIENTED_EDGE('',*,*,#4941,.F.);
#6483=ORIENTED_EDGE('',*,*,#4942,.T.);
#6484=ORIENTED_EDGE('',*,*,#4943,.F.);
#6485=ORIENTED_EDGE('',*,*,#4942,.F.);
#6486=ORIENTED_EDGE('',*,*,#4944,.F.);
#6487=ORIENTED_EDGE('',*,*,#4945,.T.);
#6488=ORIENTED_EDGE('',*,*,#4946,.F.);
#6489=ORIENTED_EDGE('',*,*,#4945,.F.);
#6490=ORIENTED_EDGE('',*,*,#4947,.F.);
#6491=ORIENTED_EDGE('',*,*,#4948,.T.);
#6492=ORIENTED_EDGE('',*,*,#4949,.T.);
#6493=ORIENTED_EDGE('',*,*,#4948,.F.);
#6494=ORIENTED_EDGE('',*,*,#4950,.F.);
#6495=ORIENTED_EDGE('',*,*,#4951,.T.);
#6496=ORIENTED_EDGE('',*,*,#4952,.T.);
#6497=ORIENTED_EDGE('',*,*,#4951,.F.);
#6498=ORIENTED_EDGE('',*,*,#4950,.T.);
#6499=ORIENTED_EDGE('',*,*,#4947,.T.);
#6500=ORIENTED_EDGE('',*,*,#4946,.T.);
#6501=ORIENTED_EDGE('',*,*,#4943,.T.);
#6502=ORIENTED_EDGE('',*,*,#4940,.T.);
#6503=ORIENTED_EDGE('',*,*,#4937,.T.);
#6504=ORIENTED_EDGE('',*,*,#4952,.F.);
#6505=ORIENTED_EDGE('',*,*,#4949,.F.);
#6506=ORIENTED_EDGE('',*,*,#4944,.T.);
#6507=ORIENTED_EDGE('',*,*,#4941,.T.);
#6508=ORIENTED_EDGE('',*,*,#4938,.T.);
#6509=ORIENTED_EDGE('',*,*,#4935,.T.);
#6510=ORIENTED_EDGE('',*,*,#4953,.F.);
#6511=ORIENTED_EDGE('',*,*,#4954,.T.);
#6512=ORIENTED_EDGE('',*,*,#4955,.F.);
#6513=ORIENTED_EDGE('',*,*,#4954,.F.);
#6514=ORIENTED_EDGE('',*,*,#4956,.F.);
#6515=ORIENTED_EDGE('',*,*,#4957,.T.);
#6516=ORIENTED_EDGE('',*,*,#4958,.F.);
#6517=ORIENTED_EDGE('',*,*,#4957,.F.);
#6518=ORIENTED_EDGE('',*,*,#4959,.F.);
#6519=ORIENTED_EDGE('',*,*,#4960,.T.);
#6520=ORIENTED_EDGE('',*,*,#4961,.F.);
#6521=ORIENTED_EDGE('',*,*,#4960,.F.);
#6522=ORIENTED_EDGE('',*,*,#4962,.F.);
#6523=ORIENTED_EDGE('',*,*,#4963,.T.);
#6524=ORIENTED_EDGE('',*,*,#4964,.F.);
#6525=ORIENTED_EDGE('',*,*,#4963,.F.);
#6526=ORIENTED_EDGE('',*,*,#4965,.F.);
#6527=ORIENTED_EDGE('',*,*,#4966,.T.);
#6528=ORIENTED_EDGE('',*,*,#4967,.T.);
#6529=ORIENTED_EDGE('',*,*,#4966,.F.);
#6530=ORIENTED_EDGE('',*,*,#4968,.F.);
#6531=ORIENTED_EDGE('',*,*,#4969,.T.);
#6532=ORIENTED_EDGE('',*,*,#4970,.T.);
#6533=ORIENTED_EDGE('',*,*,#4969,.F.);
#6534=ORIENTED_EDGE('',*,*,#4968,.T.);
#6535=ORIENTED_EDGE('',*,*,#4965,.T.);
#6536=ORIENTED_EDGE('',*,*,#4964,.T.);
#6537=ORIENTED_EDGE('',*,*,#4961,.T.);
#6538=ORIENTED_EDGE('',*,*,#4958,.T.);
#6539=ORIENTED_EDGE('',*,*,#4955,.T.);
#6540=ORIENTED_EDGE('',*,*,#4970,.F.);
#6541=ORIENTED_EDGE('',*,*,#4967,.F.);
#6542=ORIENTED_EDGE('',*,*,#4962,.T.);
#6543=ORIENTED_EDGE('',*,*,#4959,.T.);
#6544=ORIENTED_EDGE('',*,*,#4956,.T.);
#6545=ORIENTED_EDGE('',*,*,#4953,.T.);
#6546=ORIENTED_EDGE('',*,*,#4971,.F.);
#6547=ORIENTED_EDGE('',*,*,#4972,.F.);
#6548=ORIENTED_EDGE('',*,*,#4973,.F.);
#6549=ORIENTED_EDGE('',*,*,#4974,.F.);
#6550=ORIENTED_EDGE('',*,*,#4975,.F.);
#6551=ORIENTED_EDGE('',*,*,#4974,.T.);
#6552=ORIENTED_EDGE('',*,*,#4976,.F.);
#6553=ORIENTED_EDGE('',*,*,#4977,.T.);
#6554=ORIENTED_EDGE('',*,*,#4978,.F.);
#6555=ORIENTED_EDGE('',*,*,#4977,.F.);
#6556=ORIENTED_EDGE('',*,*,#4979,.F.);
#6557=ORIENTED_EDGE('',*,*,#4980,.F.);
#6558=ORIENTED_EDGE('',*,*,#4981,.F.);
#6559=ORIENTED_EDGE('',*,*,#4980,.T.);
#6560=ORIENTED_EDGE('',*,*,#4982,.T.);
#6561=ORIENTED_EDGE('',*,*,#4972,.T.);
#6562=ORIENTED_EDGE('',*,*,#4982,.F.);
#6563=ORIENTED_EDGE('',*,*,#4979,.T.);
#6564=ORIENTED_EDGE('',*,*,#4976,.T.);
#6565=ORIENTED_EDGE('',*,*,#4973,.T.);
#6566=ORIENTED_EDGE('',*,*,#4983,.F.);
#6567=ORIENTED_EDGE('',*,*,#4984,.T.);
#6568=ORIENTED_EDGE('',*,*,#4985,.F.);
#6569=ORIENTED_EDGE('',*,*,#4986,.T.);
#6570=ORIENTED_EDGE('',*,*,#4983,.T.);
#6571=ORIENTED_EDGE('',*,*,#4986,.F.);
#6572=ORIENTED_EDGE('',*,*,#4985,.T.);
#6573=ORIENTED_EDGE('',*,*,#4987,.F.);
#6574=ORIENTED_EDGE('',*,*,#4988,.F.);
#6575=ORIENTED_EDGE('',*,*,#4989,.T.);
#6576=ORIENTED_EDGE('',*,*,#4987,.T.);
#6577=ORIENTED_EDGE('',*,*,#4989,.F.);
#6578=ORIENTED_EDGE('',*,*,#4990,.F.);
#6579=ORIENTED_EDGE('',*,*,#4988,.T.);
#6580=ORIENTED_EDGE('',*,*,#4991,.F.);
#6581=ORIENTED_EDGE('',*,*,#4992,.T.);
#6582=ORIENTED_EDGE('',*,*,#4990,.T.);
#6583=ORIENTED_EDGE('',*,*,#4992,.F.);
#6584=ORIENTED_EDGE('',*,*,#4991,.T.);
#6585=ORIENTED_EDGE('',*,*,#4993,.F.);
#6586=ORIENTED_EDGE('',*,*,#4994,.F.);
#6587=ORIENTED_EDGE('',*,*,#4995,.T.);
#6588=ORIENTED_EDGE('',*,*,#4993,.T.);
#6589=ORIENTED_EDGE('',*,*,#4995,.F.);
#6590=ORIENTED_EDGE('',*,*,#4996,.F.);
#6591=ORIENTED_EDGE('',*,*,#4994,.T.);
#6592=ORIENTED_EDGE('',*,*,#4997,.F.);
#6593=ORIENTED_EDGE('',*,*,#4998,.T.);
#6594=ORIENTED_EDGE('',*,*,#4996,.T.);
#6595=ORIENTED_EDGE('',*,*,#4998,.F.);
#6596=ORIENTED_EDGE('',*,*,#4997,.T.);
#6597=ORIENTED_EDGE('',*,*,#4999,.F.);
#6598=ORIENTED_EDGE('',*,*,#4999,.T.);
#6599=ORIENTED_EDGE('',*,*,#5000,.T.);
#6600=ORIENTED_EDGE('',*,*,#4984,.F.);
#6601=ORIENTED_EDGE('',*,*,#5000,.F.);
#6602=ORIENTED_EDGE('',*,*,#4978,.T.);
#6603=ORIENTED_EDGE('',*,*,#4981,.T.);
#6604=ORIENTED_EDGE('',*,*,#4971,.T.);
#6605=ORIENTED_EDGE('',*,*,#4975,.T.);
#6606=ORIENTED_EDGE('',*,*,#5001,.F.);
#6607=ORIENTED_EDGE('',*,*,#5002,.F.);
#6608=ORIENTED_EDGE('',*,*,#5003,.F.);
#6609=ORIENTED_EDGE('',*,*,#5004,.F.);
#6610=ORIENTED_EDGE('',*,*,#5005,.F.);
#6611=ORIENTED_EDGE('',*,*,#5004,.T.);
#6612=ORIENTED_EDGE('',*,*,#5006,.F.);
#6613=ORIENTED_EDGE('',*,*,#5007,.T.);
#6614=ORIENTED_EDGE('',*,*,#5008,.F.);
#6615=ORIENTED_EDGE('',*,*,#5007,.F.);
#6616=ORIENTED_EDGE('',*,*,#5009,.F.);
#6617=ORIENTED_EDGE('',*,*,#5010,.F.);
#6618=ORIENTED_EDGE('',*,*,#5011,.F.);
#6619=ORIENTED_EDGE('',*,*,#5010,.T.);
#6620=ORIENTED_EDGE('',*,*,#5012,.F.);
#6621=ORIENTED_EDGE('',*,*,#5002,.T.);
#6622=ORIENTED_EDGE('',*,*,#5013,.F.);
#6623=ORIENTED_EDGE('',*,*,#5014,.T.);
#6624=ORIENTED_EDGE('',*,*,#5015,.F.);
#6625=ORIENTED_EDGE('',*,*,#5016,.T.);
#6626=ORIENTED_EDGE('',*,*,#5013,.T.);
#6627=ORIENTED_EDGE('',*,*,#5016,.F.);
#6628=ORIENTED_EDGE('',*,*,#5008,.T.);
#6629=ORIENTED_EDGE('',*,*,#5011,.T.);
#6630=ORIENTED_EDGE('',*,*,#5001,.T.);
#6631=ORIENTED_EDGE('',*,*,#5005,.T.);
#6632=ORIENTED_EDGE('',*,*,#5015,.T.);
#6633=ORIENTED_EDGE('',*,*,#5017,.F.);
#6634=ORIENTED_EDGE('',*,*,#5017,.T.);
#6635=ORIENTED_EDGE('',*,*,#5018,.T.);
#6636=ORIENTED_EDGE('',*,*,#5014,.F.);
#6637=ORIENTED_EDGE('',*,*,#5018,.F.);
#6638=ORIENTED_EDGE('',*,*,#5009,.T.);
#6639=ORIENTED_EDGE('',*,*,#5006,.T.);
#6640=ORIENTED_EDGE('',*,*,#5003,.T.);
#6641=ORIENTED_EDGE('',*,*,#5012,.T.);
#6642=ORIENTED_EDGE('',*,*,#5019,.T.);
#6643=ORIENTED_EDGE('',*,*,#5020,.T.);
#6644=ORIENTED_EDGE('',*,*,#5021,.T.);
#6645=ORIENTED_EDGE('',*,*,#5022,.F.);
#6646=ORIENTED_EDGE('',*,*,#5023,.T.);
#6647=ORIENTED_EDGE('',*,*,#5024,.T.);
#6648=ORIENTED_EDGE('',*,*,#5025,.T.);
#6649=ORIENTED_EDGE('',*,*,#5020,.F.);
#6650=ORIENTED_EDGE('',*,*,#5026,.T.);
#6651=ORIENTED_EDGE('',*,*,#5027,.T.);
#6652=ORIENTED_EDGE('',*,*,#5028,.T.);
#6653=ORIENTED_EDGE('',*,*,#5024,.F.);
#6654=ORIENTED_EDGE('',*,*,#5029,.T.);
#6655=ORIENTED_EDGE('',*,*,#5030,.T.);
#6656=ORIENTED_EDGE('',*,*,#5031,.T.);
#6657=ORIENTED_EDGE('',*,*,#5027,.F.);
#6658=ORIENTED_EDGE('',*,*,#5032,.T.);
#6659=ORIENTED_EDGE('',*,*,#5033,.T.);
#6660=ORIENTED_EDGE('',*,*,#5034,.T.);
#6661=ORIENTED_EDGE('',*,*,#5030,.F.);
#6662=ORIENTED_EDGE('',*,*,#5035,.T.);
#6663=ORIENTED_EDGE('',*,*,#5022,.T.);
#6664=ORIENTED_EDGE('',*,*,#5036,.T.);
#6665=ORIENTED_EDGE('',*,*,#5033,.F.);
#6666=ORIENTED_EDGE('',*,*,#5035,.F.);
#6667=ORIENTED_EDGE('',*,*,#5032,.F.);
#6668=ORIENTED_EDGE('',*,*,#5029,.F.);
#6669=ORIENTED_EDGE('',*,*,#5026,.F.);
#6670=ORIENTED_EDGE('',*,*,#5023,.F.);
#6671=ORIENTED_EDGE('',*,*,#5019,.F.);
#6672=ORIENTED_EDGE('',*,*,#5036,.F.);
#6673=ORIENTED_EDGE('',*,*,#5021,.F.);
#6674=ORIENTED_EDGE('',*,*,#5025,.F.);
#6675=ORIENTED_EDGE('',*,*,#5028,.F.);
#6676=ORIENTED_EDGE('',*,*,#5031,.F.);
#6677=ORIENTED_EDGE('',*,*,#5034,.F.);
#6678=ORIENTED_EDGE('',*,*,#5037,.F.);
#6679=ORIENTED_EDGE('',*,*,#5038,.F.);
#6680=ORIENTED_EDGE('',*,*,#5039,.F.);
#6681=ORIENTED_EDGE('',*,*,#5040,.T.);
#6682=ORIENTED_EDGE('',*,*,#5038,.T.);
#6683=ORIENTED_EDGE('',*,*,#5040,.F.);
#6684=ORIENTED_EDGE('',*,*,#5041,.F.);
#6685=ORIENTED_EDGE('',*,*,#5042,.T.);
#6686=ORIENTED_EDGE('',*,*,#5039,.T.);
#6687=ORIENTED_EDGE('',*,*,#5042,.F.);
#6688=ORIENTED_EDGE('',*,*,#5043,.F.);
#6689=ORIENTED_EDGE('',*,*,#5044,.T.);
#6690=ORIENTED_EDGE('',*,*,#5041,.T.);
#6691=ORIENTED_EDGE('',*,*,#5044,.F.);
#6692=ORIENTED_EDGE('',*,*,#5043,.T.);
#6693=ORIENTED_EDGE('',*,*,#5045,.F.);
#6694=ORIENTED_EDGE('',*,*,#5046,.F.);
#6695=ORIENTED_EDGE('',*,*,#5047,.T.);
#6696=ORIENTED_EDGE('',*,*,#5045,.T.);
#6697=ORIENTED_EDGE('',*,*,#5047,.F.);
#6698=ORIENTED_EDGE('',*,*,#5037,.T.);
#6699=ORIENTED_EDGE('',*,*,#5048,.T.);
#6700=ORIENTED_EDGE('',*,*,#5046,.T.);
#6701=ORIENTED_EDGE('',*,*,#5048,.F.);
#6702=ORIENTED_EDGE('',*,*,#5049,.T.);
#6703=ORIENTED_EDGE('',*,*,#5050,.T.);
#6704=ORIENTED_EDGE('',*,*,#5051,.T.);
#6705=ORIENTED_EDGE('',*,*,#5052,.F.);
#6706=ORIENTED_EDGE('',*,*,#5053,.T.);
#6707=ORIENTED_EDGE('',*,*,#5054,.T.);
#6708=ORIENTED_EDGE('',*,*,#5055,.T.);
#6709=ORIENTED_EDGE('',*,*,#5050,.F.);
#6710=ORIENTED_EDGE('',*,*,#5056,.T.);
#6711=ORIENTED_EDGE('',*,*,#5057,.T.);
#6712=ORIENTED_EDGE('',*,*,#5058,.T.);
#6713=ORIENTED_EDGE('',*,*,#5054,.F.);
#6714=ORIENTED_EDGE('',*,*,#5059,.T.);
#6715=ORIENTED_EDGE('',*,*,#5060,.T.);
#6716=ORIENTED_EDGE('',*,*,#5061,.T.);
#6717=ORIENTED_EDGE('',*,*,#5057,.F.);
#6718=ORIENTED_EDGE('',*,*,#5062,.T.);
#6719=ORIENTED_EDGE('',*,*,#5063,.T.);
#6720=ORIENTED_EDGE('',*,*,#5064,.T.);
#6721=ORIENTED_EDGE('',*,*,#5060,.F.);
#6722=ORIENTED_EDGE('',*,*,#5065,.T.);
#6723=ORIENTED_EDGE('',*,*,#5052,.T.);
#6724=ORIENTED_EDGE('',*,*,#5066,.T.);
#6725=ORIENTED_EDGE('',*,*,#5063,.F.);
#6726=ORIENTED_EDGE('',*,*,#5065,.F.);
#6727=ORIENTED_EDGE('',*,*,#5062,.F.);
#6728=ORIENTED_EDGE('',*,*,#5059,.F.);
#6729=ORIENTED_EDGE('',*,*,#5056,.F.);
#6730=ORIENTED_EDGE('',*,*,#5053,.F.);
#6731=ORIENTED_EDGE('',*,*,#5049,.F.);
#6732=ORIENTED_EDGE('',*,*,#5066,.F.);
#6733=ORIENTED_EDGE('',*,*,#5051,.F.);
#6734=ORIENTED_EDGE('',*,*,#5055,.F.);
#6735=ORIENTED_EDGE('',*,*,#5058,.F.);
#6736=ORIENTED_EDGE('',*,*,#5061,.F.);
#6737=ORIENTED_EDGE('',*,*,#5064,.F.);
#6738=ORIENTED_EDGE('',*,*,#5067,.T.);
#6739=ORIENTED_EDGE('',*,*,#5068,.F.);
#6740=ORIENTED_EDGE('',*,*,#5067,.F.);
#6741=ORIENTED_EDGE('',*,*,#5069,.T.);
#6742=ORIENTED_EDGE('',*,*,#5070,.T.);
#6743=ORIENTED_EDGE('',*,*,#5069,.F.);
#6744=ORIENTED_EDGE('',*,*,#5070,.F.);
#6745=ORIENTED_EDGE('',*,*,#5071,.F.);
#6746=ORIENTED_EDGE('',*,*,#5072,.F.);
#6747=ORIENTED_EDGE('',*,*,#5073,.T.);
#6748=ORIENTED_EDGE('',*,*,#5071,.T.);
#6749=ORIENTED_EDGE('',*,*,#5073,.F.);
#6750=ORIENTED_EDGE('',*,*,#5074,.F.);
#6751=ORIENTED_EDGE('',*,*,#5075,.T.);
#6752=ORIENTED_EDGE('',*,*,#5072,.T.);
#6753=ORIENTED_EDGE('',*,*,#5075,.F.);
#6754=ORIENTED_EDGE('',*,*,#5076,.F.);
#6755=ORIENTED_EDGE('',*,*,#5077,.T.);
#6756=ORIENTED_EDGE('',*,*,#5074,.T.);
#6757=ORIENTED_EDGE('',*,*,#5077,.F.);
#6758=ORIENTED_EDGE('',*,*,#5076,.T.);
#6759=ORIENTED_EDGE('',*,*,#5078,.F.);
#6760=ORIENTED_EDGE('',*,*,#5079,.F.);
#6761=ORIENTED_EDGE('',*,*,#5080,.T.);
#6762=ORIENTED_EDGE('',*,*,#5078,.T.);
#6763=ORIENTED_EDGE('',*,*,#5080,.F.);
#6764=ORIENTED_EDGE('',*,*,#5081,.F.);
#6765=ORIENTED_EDGE('',*,*,#5082,.T.);
#6766=ORIENTED_EDGE('',*,*,#5079,.T.);
#6767=ORIENTED_EDGE('',*,*,#5082,.F.);
#6768=ORIENTED_EDGE('',*,*,#5068,.T.);
#6769=ORIENTED_EDGE('',*,*,#5083,.T.);
#6770=ORIENTED_EDGE('',*,*,#5081,.T.);
#6771=ORIENTED_EDGE('',*,*,#5083,.F.);
#6772=ORIENTED_EDGE('',*,*,#5084,.F.);
#6773=ORIENTED_EDGE('',*,*,#5085,.T.);
#6774=ORIENTED_EDGE('',*,*,#5086,.F.);
#6775=ORIENTED_EDGE('',*,*,#5085,.F.);
#6776=ORIENTED_EDGE('',*,*,#5084,.T.);
#6777=ORIENTED_EDGE('',*,*,#5087,.F.);
#6778=ORIENTED_EDGE('',*,*,#5088,.F.);
#6779=ORIENTED_EDGE('',*,*,#5089,.T.);
#6780=ORIENTED_EDGE('',*,*,#5090,.T.);
#6781=ORIENTED_EDGE('',*,*,#5089,.F.);
#6782=ORIENTED_EDGE('',*,*,#5091,.F.);
#6783=ORIENTED_EDGE('',*,*,#5090,.F.);
#6784=ORIENTED_EDGE('',*,*,#5092,.F.);
#6785=ORIENTED_EDGE('',*,*,#5088,.T.);
#6786=ORIENTED_EDGE('',*,*,#5092,.T.);
#6787=ORIENTED_EDGE('',*,*,#5093,.T.);
#6788=ORIENTED_EDGE('',*,*,#5094,.T.);
#6789=ORIENTED_EDGE('',*,*,#5093,.F.);
#6790=ORIENTED_EDGE('',*,*,#5087,.T.);
#6791=ORIENTED_EDGE('',*,*,#5095,.T.);
#6792=ORIENTED_EDGE('',*,*,#5096,.T.);
#6793=ORIENTED_EDGE('',*,*,#5095,.F.);
#6794=ORIENTED_EDGE('',*,*,#5097,.F.);
#6795=ORIENTED_EDGE('',*,*,#5098,.T.);
#6796=ORIENTED_EDGE('',*,*,#5091,.T.);
#6797=ORIENTED_EDGE('',*,*,#5098,.F.);
#6798=ORIENTED_EDGE('',*,*,#5097,.T.);
#6799=ORIENTED_EDGE('',*,*,#5086,.T.);
#6800=ORIENTED_EDGE('',*,*,#5094,.F.);
#6801=ORIENTED_EDGE('',*,*,#5096,.F.);
#6802=ORIENTED_EDGE('',*,*,#5099,.F.);
#6803=ORIENTED_EDGE('',*,*,#5100,.T.);
#6804=ORIENTED_EDGE('',*,*,#5099,.T.);
#6805=ORIENTED_EDGE('',*,*,#5100,.F.);
#6806=ORIENTED_EDGE('',*,*,#5101,.F.);
#6807=ORIENTED_EDGE('',*,*,#5102,.T.);
#6808=ORIENTED_EDGE('',*,*,#5103,.F.);
#6809=ORIENTED_EDGE('',*,*,#5102,.F.);
#6810=ORIENTED_EDGE('',*,*,#5101,.T.);
#6811=ORIENTED_EDGE('',*,*,#5104,.F.);
#6812=ORIENTED_EDGE('',*,*,#5105,.T.);
#6813=ORIENTED_EDGE('',*,*,#5106,.T.);
#6814=ORIENTED_EDGE('',*,*,#5105,.F.);
#6815=ORIENTED_EDGE('',*,*,#5104,.T.);
#6816=ORIENTED_EDGE('',*,*,#5103,.T.);
#6817=ORIENTED_EDGE('',*,*,#5106,.F.);
#6818=ORIENTED_EDGE('',*,*,#5107,.F.);
#6819=ORIENTED_EDGE('',*,*,#5108,.F.);
#6820=ORIENTED_EDGE('',*,*,#5109,.T.);
#6821=ORIENTED_EDGE('',*,*,#5107,.T.);
#6822=ORIENTED_EDGE('',*,*,#5109,.F.);
#6823=ORIENTED_EDGE('',*,*,#5110,.F.);
#6824=ORIENTED_EDGE('',*,*,#5111,.T.);
#6825=ORIENTED_EDGE('',*,*,#5108,.T.);
#6826=ORIENTED_EDGE('',*,*,#5111,.F.);
#6827=ORIENTED_EDGE('',*,*,#5112,.F.);
#6828=ORIENTED_EDGE('',*,*,#5113,.T.);
#6829=ORIENTED_EDGE('',*,*,#5110,.T.);
#6830=ORIENTED_EDGE('',*,*,#5113,.F.);
#6831=ORIENTED_EDGE('',*,*,#5112,.T.);
#6832=ORIENTED_EDGE('',*,*,#5114,.F.);
#6833=ORIENTED_EDGE('',*,*,#5115,.F.);
#6834=ORIENTED_EDGE('',*,*,#5116,.T.);
#6835=ORIENTED_EDGE('',*,*,#5114,.T.);
#6836=ORIENTED_EDGE('',*,*,#5116,.F.);
#6837=ORIENTED_EDGE('',*,*,#5117,.F.);
#6838=ORIENTED_EDGE('',*,*,#5118,.T.);
#6839=ORIENTED_EDGE('',*,*,#5115,.T.);
#6840=ORIENTED_EDGE('',*,*,#5118,.F.);
#6841=ORIENTED_EDGE('',*,*,#5119,.F.);
#6842=ORIENTED_EDGE('',*,*,#5120,.T.);
#6843=ORIENTED_EDGE('',*,*,#5117,.T.);
#6844=ORIENTED_EDGE('',*,*,#5120,.F.);
#6845=ORIENTED_EDGE('',*,*,#5119,.T.);
#6846=ORIENTED_EDGE('',*,*,#5121,.T.);
#6847=ORIENTED_EDGE('',*,*,#5122,.T.);
#6848=ORIENTED_EDGE('',*,*,#5123,.T.);
#6849=ORIENTED_EDGE('',*,*,#5124,.F.);
#6850=ORIENTED_EDGE('',*,*,#5125,.T.);
#6851=ORIENTED_EDGE('',*,*,#5126,.T.);
#6852=ORIENTED_EDGE('',*,*,#5127,.T.);
#6853=ORIENTED_EDGE('',*,*,#5122,.F.);
#6854=ORIENTED_EDGE('',*,*,#5128,.T.);
#6855=ORIENTED_EDGE('',*,*,#5129,.T.);
#6856=ORIENTED_EDGE('',*,*,#5130,.T.);
#6857=ORIENTED_EDGE('',*,*,#5126,.F.);
#6858=ORIENTED_EDGE('',*,*,#5131,.T.);
#6859=ORIENTED_EDGE('',*,*,#5132,.T.);
#6860=ORIENTED_EDGE('',*,*,#5133,.T.);
#6861=ORIENTED_EDGE('',*,*,#5129,.F.);
#6862=ORIENTED_EDGE('',*,*,#5134,.T.);
#6863=ORIENTED_EDGE('',*,*,#5135,.T.);
#6864=ORIENTED_EDGE('',*,*,#5136,.T.);
#6865=ORIENTED_EDGE('',*,*,#5132,.F.);
#6866=ORIENTED_EDGE('',*,*,#5137,.T.);
#6867=ORIENTED_EDGE('',*,*,#5124,.T.);
#6868=ORIENTED_EDGE('',*,*,#5138,.T.);
#6869=ORIENTED_EDGE('',*,*,#5135,.F.);
#6870=ORIENTED_EDGE('',*,*,#5137,.F.);
#6871=ORIENTED_EDGE('',*,*,#5134,.F.);
#6872=ORIENTED_EDGE('',*,*,#5131,.F.);
#6873=ORIENTED_EDGE('',*,*,#5128,.F.);
#6874=ORIENTED_EDGE('',*,*,#5125,.F.);
#6875=ORIENTED_EDGE('',*,*,#5121,.F.);
#6876=ORIENTED_EDGE('',*,*,#5138,.F.);
#6877=ORIENTED_EDGE('',*,*,#5123,.F.);
#6878=ORIENTED_EDGE('',*,*,#5127,.F.);
#6879=ORIENTED_EDGE('',*,*,#5130,.F.);
#6880=ORIENTED_EDGE('',*,*,#5133,.F.);
#6881=ORIENTED_EDGE('',*,*,#5136,.F.);
#6882=ORIENTED_EDGE('',*,*,#5139,.F.);
#6883=ORIENTED_EDGE('',*,*,#5140,.T.);
#6884=ORIENTED_EDGE('',*,*,#5141,.F.);
#6885=ORIENTED_EDGE('',*,*,#5140,.F.);
#6886=ORIENTED_EDGE('',*,*,#5142,.F.);
#6887=ORIENTED_EDGE('',*,*,#5143,.T.);
#6888=ORIENTED_EDGE('',*,*,#5144,.F.);
#6889=ORIENTED_EDGE('',*,*,#5143,.F.);
#6890=ORIENTED_EDGE('',*,*,#5145,.F.);
#6891=ORIENTED_EDGE('',*,*,#5146,.T.);
#6892=ORIENTED_EDGE('',*,*,#5147,.F.);
#6893=ORIENTED_EDGE('',*,*,#5148,.F.);
#6894=ORIENTED_EDGE('',*,*,#5149,.T.);
#6895=ORIENTED_EDGE('',*,*,#5150,.F.);
#6896=ORIENTED_EDGE('',*,*,#5149,.F.);
#6897=ORIENTED_EDGE('',*,*,#5151,.F.);
#6898=ORIENTED_EDGE('',*,*,#5152,.F.);
#6899=ORIENTED_EDGE('',*,*,#5146,.F.);
#6900=ORIENTED_EDGE('',*,*,#5153,.F.);
#6901=ORIENTED_EDGE('',*,*,#5151,.T.);
#6902=ORIENTED_EDGE('',*,*,#5148,.T.);
#6903=ORIENTED_EDGE('',*,*,#5154,.F.);
#6904=ORIENTED_EDGE('',*,*,#5155,.T.);
#6905=ORIENTED_EDGE('',*,*,#5156,.F.);
#6906=ORIENTED_EDGE('',*,*,#5155,.F.);
#6907=ORIENTED_EDGE('',*,*,#5152,.T.);
#6908=ORIENTED_EDGE('',*,*,#5153,.T.);
#6909=ORIENTED_EDGE('',*,*,#5147,.T.);
#6910=ORIENTED_EDGE('',*,*,#5145,.T.);
#6911=ORIENTED_EDGE('',*,*,#5157,.F.);
#6912=ORIENTED_EDGE('',*,*,#5158,.F.);
#6913=ORIENTED_EDGE('',*,*,#5159,.F.);
#6914=ORIENTED_EDGE('',*,*,#5160,.F.);
#6915=ORIENTED_EDGE('',*,*,#5142,.T.);
#6916=ORIENTED_EDGE('',*,*,#5161,.F.);
#6917=ORIENTED_EDGE('',*,*,#5162,.F.);
#6918=ORIENTED_EDGE('',*,*,#5163,.F.);
#6919=ORIENTED_EDGE('',*,*,#5158,.T.);
#6920=ORIENTED_EDGE('',*,*,#5154,.T.);
#6921=ORIENTED_EDGE('',*,*,#5164,.F.);
#6922=ORIENTED_EDGE('',*,*,#5165,.F.);
#6923=ORIENTED_EDGE('',*,*,#5166,.F.);
#6924=ORIENTED_EDGE('',*,*,#5162,.T.);
#6925=ORIENTED_EDGE('',*,*,#5141,.T.);
#6926=ORIENTED_EDGE('',*,*,#5159,.T.);
#6927=ORIENTED_EDGE('',*,*,#5163,.T.);
#6928=ORIENTED_EDGE('',*,*,#5166,.T.);
#6929=ORIENTED_EDGE('',*,*,#5167,.F.);
#6930=ORIENTED_EDGE('',*,*,#5168,.F.);
#6931=ORIENTED_EDGE('',*,*,#5169,.F.);
#6932=ORIENTED_EDGE('',*,*,#5170,.F.);
#6933=ORIENTED_EDGE('',*,*,#5171,.F.);
#6934=ORIENTED_EDGE('',*,*,#5165,.T.);
#6935=ORIENTED_EDGE('',*,*,#5172,.F.);
#6936=ORIENTED_EDGE('',*,*,#5173,.F.);
#6937=ORIENTED_EDGE('',*,*,#5167,.T.);
#6938=ORIENTED_EDGE('',*,*,#5160,.T.);
#6939=ORIENTED_EDGE('',*,*,#5171,.T.);
#6940=ORIENTED_EDGE('',*,*,#5174,.T.);
#6941=ORIENTED_EDGE('',*,*,#5175,.F.);
#6942=ORIENTED_EDGE('',*,*,#5169,.T.);
#6943=ORIENTED_EDGE('',*,*,#5176,.T.);
#6944=ORIENTED_EDGE('',*,*,#5177,.F.);
#6945=ORIENTED_EDGE('',*,*,#5178,.F.);
#6946=ORIENTED_EDGE('',*,*,#5156,.T.);
#6947=ORIENTED_EDGE('',*,*,#5170,.T.);
#6948=ORIENTED_EDGE('',*,*,#5178,.T.);
#6949=ORIENTED_EDGE('',*,*,#5179,.F.);
#6950=ORIENTED_EDGE('',*,*,#5174,.F.);
#6951=ORIENTED_EDGE('',*,*,#5144,.T.);
#6952=ORIENTED_EDGE('',*,*,#5168,.T.);
#6953=ORIENTED_EDGE('',*,*,#5173,.T.);
#6954=ORIENTED_EDGE('',*,*,#5180,.F.);
#6955=ORIENTED_EDGE('',*,*,#5176,.F.);
#6956=ORIENTED_EDGE('',*,*,#5139,.T.);
#6957=ORIENTED_EDGE('',*,*,#5157,.T.);
#6958=ORIENTED_EDGE('',*,*,#5175,.T.);
#6959=ORIENTED_EDGE('',*,*,#5179,.T.);
#6960=ORIENTED_EDGE('',*,*,#5177,.T.);
#6961=ORIENTED_EDGE('',*,*,#5180,.T.);
#6962=ORIENTED_EDGE('',*,*,#5172,.T.);
#6963=ORIENTED_EDGE('',*,*,#5164,.T.);
#6964=ORIENTED_EDGE('',*,*,#5161,.T.);
#6965=ORIENTED_EDGE('',*,*,#5150,.T.);
#6966=ORIENTED_EDGE('',*,*,#5181,.F.);
#6967=ORIENTED_EDGE('',*,*,#5182,.T.);
#6968=ORIENTED_EDGE('',*,*,#5183,.T.);
#6969=ORIENTED_EDGE('',*,*,#5184,.F.);
#6970=ORIENTED_EDGE('',*,*,#5185,.F.);
#6971=ORIENTED_EDGE('',*,*,#5186,.T.);
#6972=ORIENTED_EDGE('',*,*,#5187,.T.);
#6973=ORIENTED_EDGE('',*,*,#5182,.F.);
#6974=ORIENTED_EDGE('',*,*,#5188,.F.);
#6975=ORIENTED_EDGE('',*,*,#5189,.T.);
#6976=ORIENTED_EDGE('',*,*,#5190,.T.);
#6977=ORIENTED_EDGE('',*,*,#5186,.F.);
#6978=ORIENTED_EDGE('',*,*,#5191,.F.);
#6979=ORIENTED_EDGE('',*,*,#5192,.T.);
#6980=ORIENTED_EDGE('',*,*,#5193,.T.);
#6981=ORIENTED_EDGE('',*,*,#5189,.F.);
#6982=ORIENTED_EDGE('',*,*,#5194,.F.);
#6983=ORIENTED_EDGE('',*,*,#5195,.T.);
#6984=ORIENTED_EDGE('',*,*,#5196,.T.);
#6985=ORIENTED_EDGE('',*,*,#5192,.F.);
#6986=ORIENTED_EDGE('',*,*,#5197,.F.);
#6987=ORIENTED_EDGE('',*,*,#5184,.T.);
#6988=ORIENTED_EDGE('',*,*,#5198,.T.);
#6989=ORIENTED_EDGE('',*,*,#5195,.F.);
#6990=ORIENTED_EDGE('',*,*,#5198,.F.);
#6991=ORIENTED_EDGE('',*,*,#5183,.F.);
#6992=ORIENTED_EDGE('',*,*,#5187,.F.);
#6993=ORIENTED_EDGE('',*,*,#5190,.F.);
#6994=ORIENTED_EDGE('',*,*,#5193,.F.);
#6995=ORIENTED_EDGE('',*,*,#5196,.F.);
#6996=ORIENTED_EDGE('',*,*,#5199,.F.);
#6997=ORIENTED_EDGE('',*,*,#5181,.T.);
#6998=ORIENTED_EDGE('',*,*,#5197,.T.);
#6999=ORIENTED_EDGE('',*,*,#5194,.T.);
#7000=ORIENTED_EDGE('',*,*,#5191,.T.);
#7001=ORIENTED_EDGE('',*,*,#5188,.T.);
#7002=ORIENTED_EDGE('',*,*,#5185,.T.);
#7003=ORIENTED_EDGE('',*,*,#5200,.F.);
#7004=ORIENTED_EDGE('',*,*,#5201,.T.);
#7005=ORIENTED_EDGE('',*,*,#5199,.T.);
#7006=ORIENTED_EDGE('',*,*,#5201,.F.);
#7007=ORIENTED_EDGE('',*,*,#5202,.F.);
#7008=ORIENTED_EDGE('',*,*,#5203,.T.);
#7009=ORIENTED_EDGE('',*,*,#5200,.T.);
#7010=ORIENTED_EDGE('',*,*,#5203,.F.);
#7011=ORIENTED_EDGE('',*,*,#5204,.F.);
#7012=ORIENTED_EDGE('',*,*,#5205,.T.);
#7013=ORIENTED_EDGE('',*,*,#5202,.T.);
#7014=ORIENTED_EDGE('',*,*,#5205,.F.);
#7015=ORIENTED_EDGE('',*,*,#5204,.T.);
#7016=ORIENTED_EDGE('',*,*,#5206,.F.);
#7017=ORIENTED_EDGE('',*,*,#5207,.T.);
#7018=ORIENTED_EDGE('',*,*,#5208,.F.);
#7019=ORIENTED_EDGE('',*,*,#5207,.F.);
#7020=ORIENTED_EDGE('',*,*,#5209,.F.);
#7021=ORIENTED_EDGE('',*,*,#5210,.F.);
#7022=ORIENTED_EDGE('',*,*,#5211,.F.);
#7023=ORIENTED_EDGE('',*,*,#5212,.F.);
#7024=ORIENTED_EDGE('',*,*,#5213,.T.);
#7025=ORIENTED_EDGE('',*,*,#5211,.T.);
#7026=ORIENTED_EDGE('',*,*,#5213,.F.);
#7027=ORIENTED_EDGE('',*,*,#5214,.F.);
#7028=ORIENTED_EDGE('',*,*,#5215,.T.);
#7029=ORIENTED_EDGE('',*,*,#5212,.T.);
#7030=ORIENTED_EDGE('',*,*,#5215,.F.);
#7031=ORIENTED_EDGE('',*,*,#5214,.T.);
#7032=ORIENTED_EDGE('',*,*,#5216,.F.);
#7033=ORIENTED_EDGE('',*,*,#5217,.F.);
#7034=ORIENTED_EDGE('',*,*,#5218,.T.);
#7035=ORIENTED_EDGE('',*,*,#5210,.T.);
#7036=ORIENTED_EDGE('',*,*,#5219,.T.);
#7037=ORIENTED_EDGE('',*,*,#5216,.T.);
#7038=ORIENTED_EDGE('',*,*,#5219,.F.);
#7039=ORIENTED_EDGE('',*,*,#5209,.T.);
#7040=ORIENTED_EDGE('',*,*,#5206,.T.);
#7041=ORIENTED_EDGE('',*,*,#5218,.F.);
#7042=ORIENTED_EDGE('',*,*,#5208,.T.);
#7043=ORIENTED_EDGE('',*,*,#5220,.F.);
#7044=ORIENTED_EDGE('',*,*,#5221,.T.);
#7045=ORIENTED_EDGE('',*,*,#5217,.T.);
#7046=ORIENTED_EDGE('',*,*,#5221,.F.);
#7047=ORIENTED_EDGE('',*,*,#5220,.T.);
#7048=ORIENTED_EDGE('',*,*,#5222,.F.);
#7049=ORIENTED_EDGE('',*,*,#5223,.T.);
#7050=ORIENTED_EDGE('',*,*,#5224,.T.);
#7051=ORIENTED_EDGE('',*,*,#5223,.F.);
#7052=ORIENTED_EDGE('',*,*,#5225,.F.);
#7053=ORIENTED_EDGE('',*,*,#5226,.T.);
#7054=ORIENTED_EDGE('',*,*,#5227,.T.);
#7055=ORIENTED_EDGE('',*,*,#5226,.F.);
#7056=ORIENTED_EDGE('',*,*,#5225,.T.);
#7057=ORIENTED_EDGE('',*,*,#5222,.T.);
#7058=ORIENTED_EDGE('',*,*,#5227,.F.);
#7059=ORIENTED_EDGE('',*,*,#5224,.F.);
#7060=ORIENTED_EDGE('',*,*,#5228,.F.);
#7061=ORIENTED_EDGE('',*,*,#5229,.T.);
#7062=ORIENTED_EDGE('',*,*,#5228,.T.);
#7063=ORIENTED_EDGE('',*,*,#5229,.F.);
#7064=ORIENTED_EDGE('',*,*,#5230,.F.);
#7065=ORIENTED_EDGE('',*,*,#5231,.F.);
#7066=ORIENTED_EDGE('',*,*,#5232,.T.);
#7067=ORIENTED_EDGE('',*,*,#5233,.F.);
#7068=ORIENTED_EDGE('',*,*,#5233,.T.);
#7069=ORIENTED_EDGE('',*,*,#5234,.T.);
#7070=ORIENTED_EDGE('',*,*,#5235,.F.);
#7071=ORIENTED_EDGE('',*,*,#5236,.F.);
#7072=ORIENTED_EDGE('',*,*,#5232,.F.);
#7073=ORIENTED_EDGE('',*,*,#5236,.T.);
#7074=ORIENTED_EDGE('',*,*,#5237,.F.);
#7075=ORIENTED_EDGE('',*,*,#5238,.T.);
#7076=ORIENTED_EDGE('',*,*,#5231,.T.);
#7077=ORIENTED_EDGE('',*,*,#5230,.T.);
#7078=ORIENTED_EDGE('',*,*,#5238,.F.);
#7079=ORIENTED_EDGE('',*,*,#5239,.F.);
#7080=ORIENTED_EDGE('',*,*,#5234,.F.);
#7081=ORIENTED_EDGE('',*,*,#5239,.T.);
#7082=ORIENTED_EDGE('',*,*,#5237,.T.);
#7083=ORIENTED_EDGE('',*,*,#5235,.T.);
#7084=ORIENTED_EDGE('',*,*,#5240,.F.);
#7085=ORIENTED_EDGE('',*,*,#5241,.T.);
#7086=ORIENTED_EDGE('',*,*,#5242,.T.);
#7087=ORIENTED_EDGE('',*,*,#5241,.F.);
#7088=ORIENTED_EDGE('',*,*,#5242,.F.);
#7089=ORIENTED_EDGE('',*,*,#5243,.F.);
#7090=ORIENTED_EDGE('',*,*,#5244,.T.);
#7091=ORIENTED_EDGE('',*,*,#5245,.T.);
#7092=ORIENTED_EDGE('',*,*,#5244,.F.);
#7093=ORIENTED_EDGE('',*,*,#5243,.T.);
#7094=ORIENTED_EDGE('',*,*,#5245,.F.);
#7095=ORIENTED_EDGE('',*,*,#5240,.T.);
#7096=ORIENTED_EDGE('',*,*,#5246,.F.);
#7097=ORIENTED_EDGE('',*,*,#5247,.T.);
#7098=ORIENTED_EDGE('',*,*,#5248,.T.);
#7099=ORIENTED_EDGE('',*,*,#5247,.F.);
#7100=ORIENTED_EDGE('',*,*,#5248,.F.);
#7101=ORIENTED_EDGE('',*,*,#5249,.F.);
#7102=ORIENTED_EDGE('',*,*,#5250,.T.);
#7103=ORIENTED_EDGE('',*,*,#5251,.T.);
#7104=ORIENTED_EDGE('',*,*,#5250,.F.);
#7105=ORIENTED_EDGE('',*,*,#5249,.T.);
#7106=ORIENTED_EDGE('',*,*,#5251,.F.);
#7107=ORIENTED_EDGE('',*,*,#5246,.T.);
#7108=ORIENTED_EDGE('',*,*,#5252,.F.);
#7109=ORIENTED_EDGE('',*,*,#5253,.T.);
#7110=ORIENTED_EDGE('',*,*,#5254,.F.);
#7111=ORIENTED_EDGE('',*,*,#5253,.F.);
#7112=ORIENTED_EDGE('',*,*,#5255,.F.);
#7113=ORIENTED_EDGE('',*,*,#5256,.T.);
#7114=ORIENTED_EDGE('',*,*,#5257,.F.);
#7115=ORIENTED_EDGE('',*,*,#5256,.F.);
#7116=ORIENTED_EDGE('',*,*,#5258,.F.);
#7117=ORIENTED_EDGE('',*,*,#5259,.T.);
#7118=ORIENTED_EDGE('',*,*,#5260,.F.);
#7119=ORIENTED_EDGE('',*,*,#5259,.F.);
#7120=ORIENTED_EDGE('',*,*,#5261,.F.);
#7121=ORIENTED_EDGE('',*,*,#5262,.F.);
#7122=ORIENTED_EDGE('',*,*,#5263,.F.);
#7123=ORIENTED_EDGE('',*,*,#5264,.F.);
#7124=ORIENTED_EDGE('',*,*,#5265,.F.);
#7125=ORIENTED_EDGE('',*,*,#5266,.F.);
#7126=ORIENTED_EDGE('',*,*,#5267,.F.);
#7127=ORIENTED_EDGE('',*,*,#5262,.T.);
#7128=ORIENTED_EDGE('',*,*,#5258,.T.);
#7129=ORIENTED_EDGE('',*,*,#5263,.T.);
#7130=ORIENTED_EDGE('',*,*,#5267,.T.);
#7131=ORIENTED_EDGE('',*,*,#5268,.F.);
#7132=ORIENTED_EDGE('',*,*,#5269,.F.);
#7133=ORIENTED_EDGE('',*,*,#5270,.F.);
#7134=ORIENTED_EDGE('',*,*,#5264,.T.);
#7135=ORIENTED_EDGE('',*,*,#5269,.T.);
#7136=ORIENTED_EDGE('',*,*,#5271,.F.);
#7137=ORIENTED_EDGE('',*,*,#5260,.T.);
#7138=ORIENTED_EDGE('',*,*,#5272,.F.);
#7139=ORIENTED_EDGE('',*,*,#5271,.T.);
#7140=ORIENTED_EDGE('',*,*,#5268,.T.);
#7141=ORIENTED_EDGE('',*,*,#5266,.T.);
#7142=ORIENTED_EDGE('',*,*,#5273,.T.);
#7143=ORIENTED_EDGE('',*,*,#5274,.T.);
#7144=ORIENTED_EDGE('',*,*,#5275,.F.);
#7145=ORIENTED_EDGE('',*,*,#5276,.F.);
#7146=ORIENTED_EDGE('',*,*,#5254,.T.);
#7147=ORIENTED_EDGE('',*,*,#5257,.T.);
#7148=ORIENTED_EDGE('',*,*,#5265,.T.);
#7149=ORIENTED_EDGE('',*,*,#5261,.T.);
#7150=ORIENTED_EDGE('',*,*,#5270,.T.);
#7151=ORIENTED_EDGE('',*,*,#5272,.T.);
#7152=ORIENTED_EDGE('',*,*,#5277,.T.);
#7153=ORIENTED_EDGE('',*,*,#5276,.T.);
#7154=ORIENTED_EDGE('',*,*,#5278,.F.);
#7155=ORIENTED_EDGE('',*,*,#5279,.F.);
#7156=ORIENTED_EDGE('',*,*,#5280,.T.);
#7157=ORIENTED_EDGE('',*,*,#5279,.T.);
#7158=ORIENTED_EDGE('',*,*,#5281,.F.);
#7159=ORIENTED_EDGE('',*,*,#5282,.F.);
#7160=ORIENTED_EDGE('',*,*,#5252,.T.);
#7161=ORIENTED_EDGE('',*,*,#5255,.T.);
#7162=ORIENTED_EDGE('',*,*,#5283,.T.);
#7163=ORIENTED_EDGE('',*,*,#5282,.T.);
#7164=ORIENTED_EDGE('',*,*,#5284,.F.);
#7165=ORIENTED_EDGE('',*,*,#5274,.F.);
#7166=ORIENTED_EDGE('',*,*,#5284,.T.);
#7167=ORIENTED_EDGE('',*,*,#5281,.T.);
#7168=ORIENTED_EDGE('',*,*,#5278,.T.);
#7169=ORIENTED_EDGE('',*,*,#5275,.T.);
#7170=ORIENTED_EDGE('',*,*,#5283,.F.);
#7171=ORIENTED_EDGE('',*,*,#5273,.F.);
#7172=ORIENTED_EDGE('',*,*,#5277,.F.);
#7173=ORIENTED_EDGE('',*,*,#5280,.F.);
#7174=ORIENTED_EDGE('',*,*,#5285,.F.);
#7175=ORIENTED_EDGE('',*,*,#5286,.T.);
#7176=ORIENTED_EDGE('',*,*,#5287,.T.);
#7177=ORIENTED_EDGE('',*,*,#5286,.F.);
#7178=ORIENTED_EDGE('',*,*,#5288,.F.);
#7179=ORIENTED_EDGE('',*,*,#5289,.T.);
#7180=ORIENTED_EDGE('',*,*,#5290,.T.);
#7181=ORIENTED_EDGE('',*,*,#5289,.F.);
#7182=ORIENTED_EDGE('',*,*,#5288,.T.);
#7183=ORIENTED_EDGE('',*,*,#5285,.T.);
#7184=ORIENTED_EDGE('',*,*,#5290,.F.);
#7185=ORIENTED_EDGE('',*,*,#5287,.F.);
#7186=ORIENTED_EDGE('',*,*,#5291,.F.);
#7187=ORIENTED_EDGE('',*,*,#5292,.F.);
#7188=ORIENTED_EDGE('',*,*,#5293,.T.);
#7189=ORIENTED_EDGE('',*,*,#5294,.F.);
#7190=ORIENTED_EDGE('',*,*,#5293,.F.);
#7191=ORIENTED_EDGE('',*,*,#5295,.F.);
#7192=ORIENTED_EDGE('',*,*,#5296,.F.);
#7193=ORIENTED_EDGE('',*,*,#5297,.F.);
#7194=ORIENTED_EDGE('',*,*,#5298,.F.);
#7195=ORIENTED_EDGE('',*,*,#5299,.F.);
#7196=ORIENTED_EDGE('',*,*,#5300,.T.);
#7197=ORIENTED_EDGE('',*,*,#5301,.F.);
#7198=ORIENTED_EDGE('',*,*,#5302,.F.);
#7199=ORIENTED_EDGE('',*,*,#5303,.F.);
#7200=ORIENTED_EDGE('',*,*,#5304,.F.);
#7201=ORIENTED_EDGE('',*,*,#5305,.F.);
#7202=ORIENTED_EDGE('',*,*,#5306,.F.);
#7203=ORIENTED_EDGE('',*,*,#5300,.F.);
#7204=ORIENTED_EDGE('',*,*,#5296,.T.);
#7205=ORIENTED_EDGE('',*,*,#5307,.T.);
#7206=ORIENTED_EDGE('',*,*,#5305,.T.);
#7207=ORIENTED_EDGE('',*,*,#5308,.F.);
#7208=ORIENTED_EDGE('',*,*,#5295,.T.);
#7209=ORIENTED_EDGE('',*,*,#5309,.T.);
#7210=ORIENTED_EDGE('',*,*,#5306,.T.);
#7211=ORIENTED_EDGE('',*,*,#5307,.F.);
#7212=ORIENTED_EDGE('',*,*,#5292,.T.);
#7213=ORIENTED_EDGE('',*,*,#5310,.T.);
#7214=ORIENTED_EDGE('',*,*,#5301,.T.);
#7215=ORIENTED_EDGE('',*,*,#5309,.F.);
#7216=ORIENTED_EDGE('',*,*,#5311,.F.);
#7217=ORIENTED_EDGE('',*,*,#5312,.T.);
#7218=ORIENTED_EDGE('',*,*,#5313,.T.);
#7219=ORIENTED_EDGE('',*,*,#5312,.F.);
#7220=ORIENTED_EDGE('',*,*,#5291,.T.);
#7221=ORIENTED_EDGE('',*,*,#5314,.T.);
#7222=ORIENTED_EDGE('',*,*,#5302,.T.);
#7223=ORIENTED_EDGE('',*,*,#5310,.F.);
#7224=ORIENTED_EDGE('',*,*,#5297,.T.);
#7225=ORIENTED_EDGE('',*,*,#5308,.T.);
#7226=ORIENTED_EDGE('',*,*,#5304,.T.);
#7227=ORIENTED_EDGE('',*,*,#5315,.F.);
#7228=ORIENTED_EDGE('',*,*,#5298,.T.);
#7229=ORIENTED_EDGE('',*,*,#5315,.T.);
#7230=ORIENTED_EDGE('',*,*,#5303,.T.);
#7231=ORIENTED_EDGE('',*,*,#5314,.F.);
#7232=ORIENTED_EDGE('',*,*,#5299,.T.);
#7233=ORIENTED_EDGE('',*,*,#5311,.T.);
#7234=ORIENTED_EDGE('',*,*,#5294,.T.);
#7235=ORIENTED_EDGE('',*,*,#5313,.F.);
#7236=CYLINDRICAL_SURFACE('',#8387,0.21);
#7237=CYLINDRICAL_SURFACE('',#8391,0.21);
#7238=CYLINDRICAL_SURFACE('',#8399,0.2);
#7239=CYLINDRICAL_SURFACE('',#8402,0.2);
#7240=CYLINDRICAL_SURFACE('',#8409,0.2);
#7241=CYLINDRICAL_SURFACE('',#8420,0.2);
#7242=CYLINDRICAL_SURFACE('',#8421,0.2);
#7243=CYLINDRICAL_SURFACE('',#8423,0.2);
#7244=CYLINDRICAL_SURFACE('',#8425,1.);
#7245=CYLINDRICAL_SURFACE('',#8430,0.685);
#7246=CYLINDRICAL_SURFACE('',#8434,0.275);
#7247=CYLINDRICAL_SURFACE('',#8437,0.275);
#7248=CYLINDRICAL_SURFACE('',#8440,0.275);
#7249=CYLINDRICAL_SURFACE('',#8443,0.275);
#7250=CYLINDRICAL_SURFACE('',#8446,0.6);
#7251=CYLINDRICAL_SURFACE('',#8457,0.515);
#7252=CYLINDRICAL_SURFACE('',#8464,0.4);
#7253=CYLINDRICAL_SURFACE('',#8466,0.49);
#7254=CYLINDRICAL_SURFACE('',#8473,0.25);
#7255=CYLINDRICAL_SURFACE('',#8474,0.25);
#7256=CYLINDRICAL_SURFACE('',#8495,0.2);
#7257=CYLINDRICAL_SURFACE('',#8497,0.685);
#7258=CYLINDRICAL_SURFACE('',#8505,0.3);
#7259=CYLINDRICAL_SURFACE('',#8509,0.6);
#7260=CYLINDRICAL_SURFACE('',#8513,0.21);
#7261=CYLINDRICAL_SURFACE('',#8517,0.21);
#7262=CYLINDRICAL_SURFACE('',#8527,0.2);
#7263=CYLINDRICAL_SURFACE('',#8534,0.2);
#7264=CYLINDRICAL_SURFACE('',#8537,0.2);
#7265=CYLINDRICAL_SURFACE('',#8548,0.2);
#7266=CYLINDRICAL_SURFACE('',#8549,0.2);
#7267=CYLINDRICAL_SURFACE('',#8550,0.2);
#7268=CYLINDRICAL_SURFACE('',#8555,0.685);
#7269=CYLINDRICAL_SURFACE('',#8559,0.275);
#7270=CYLINDRICAL_SURFACE('',#8562,0.275);
#7271=CYLINDRICAL_SURFACE('',#8565,0.275);
#7272=CYLINDRICAL_SURFACE('',#8568,0.275);
#7273=CYLINDRICAL_SURFACE('',#8571,1.);
#7274=CYLINDRICAL_SURFACE('',#8580,0.515);
#7275=CYLINDRICAL_SURFACE('',#8587,0.4);
#7276=CYLINDRICAL_SURFACE('',#8589,0.49);
#7277=CYLINDRICAL_SURFACE('',#8596,0.25);
#7278=CYLINDRICAL_SURFACE('',#8597,0.25);
#7279=CYLINDRICAL_SURFACE('',#8618,0.2);
#7280=CYLINDRICAL_SURFACE('',#8620,0.685);
#7281=CYLINDRICAL_SURFACE('',#8628,0.3);
#7282=CYLINDRICAL_SURFACE('',#8632,0.6);
#7283=CYLINDRICAL_SURFACE('',#8636,1.);
#7284=CYLINDRICAL_SURFACE('',#8639,1.6);
#7285=CYLINDRICAL_SURFACE('',#8645,1.);
#7286=CYLINDRICAL_SURFACE('',#8648,1.6);
#7287=CYLINDRICAL_SURFACE('',#8654,1.);
#7288=CYLINDRICAL_SURFACE('',#8657,1.6);
#7289=CYLINDRICAL_SURFACE('',#8663,0.45);
#7290=CYLINDRICAL_SURFACE('',#8668,0.45);
#7291=CYLINDRICAL_SURFACE('',#8673,0.275);
#7292=CYLINDRICAL_SURFACE('',#8675,0.275);
#7293=CYLINDRICAL_SURFACE('',#8677,0.5);
#7294=CYLINDRICAL_SURFACE('',#8682,0.5);
#7295=CYLINDRICAL_SURFACE('',#8687,0.275);
#7296=CYLINDRICAL_SURFACE('',#8689,0.275);
#7297=CYLINDRICAL_SURFACE('',#8702,0.425);
#7298=CYLINDRICAL_SURFACE('',#8710,0.24505);
#7299=CYLINDRICAL_SURFACE('',#8725,0.43);
#7300=CYLINDRICAL_SURFACE('',#8742,0.46);
#7301=CYLINDRICAL_SURFACE('',#8746,0.525);
#7302=CYLINDRICAL_SURFACE('',#8747,0.515);
#7303=CYLINDRICAL_SURFACE('',#8751,0.2);
#7304=CYLINDRICAL_SURFACE('',#8756,0.475);
#7305=CYLINDRICAL_SURFACE('',#8760,0.355);
#7306=CYLINDRICAL_SURFACE('',#8764,0.31);
#7307=CYLINDRICAL_SURFACE('',#8772,0.51);
#7308=CYLINDRICAL_SURFACE('',#8779,0.405);
#7309=CYLINDRICAL_SURFACE('',#8781,0.405);
#7310=CYLINDRICAL_SURFACE('',#8783,0.6);
#7311=CYLINDRICAL_SURFACE('',#8793,0.25);
#7312=CYLINDRICAL_SURFACE('',#8802,0.265);
#7313=CYLINDRICAL_SURFACE('',#8806,0.5);
#7314=CYLINDRICAL_SURFACE('',#8817,0.2117);
#7315=CYLINDRICAL_SURFACE('',#8826,0.33);
#7316=CYLINDRICAL_SURFACE('',#8829,0.33);
#7317=CYLINDRICAL_SURFACE('',#8832,0.33);
#7318=CYLINDRICAL_SURFACE('',#8835,0.33);
#7319=CYLINDRICAL_SURFACE('',#8838,0.21);
#7320=CYLINDRICAL_SURFACE('',#8841,0.21);
#7321=CYLINDRICAL_SURFACE('',#8844,0.21);
#7322=CYLINDRICAL_SURFACE('',#8847,0.21);
#7323=CYLINDRICAL_SURFACE('',#8850,0.165);
#7324=CYLINDRICAL_SURFACE('',#8853,0.165);
#7325=CYLINDRICAL_SURFACE('',#8856,0.165);
#7326=CYLINDRICAL_SURFACE('',#8859,0.165);
#7327=CYLINDRICAL_SURFACE('',#8862,1.05);
#7328=CYLINDRICAL_SURFACE('',#8870,0.165);
#7329=CYLINDRICAL_SURFACE('',#8873,0.165);
#7330=CYLINDRICAL_SURFACE('',#8876,0.165);
#7331=CYLINDRICAL_SURFACE('',#8879,0.165);
#7332=CYLINDRICAL_SURFACE('',#8882,1.05);
#7333=CYLINDRICAL_SURFACE('',#8897,0.225);
#7334=CYLINDRICAL_SURFACE('',#8900,0.225);
#7335=CYLINDRICAL_SURFACE('',#8903,0.225);
#7336=CYLINDRICAL_SURFACE('',#8906,0.225);
#7337=CYLINDRICAL_SURFACE('',#8909,0.62);
#7338=CYLINDRICAL_SURFACE('',#8912,2.);
#7339=CYLINDRICAL_SURFACE('',#8918,0.225);
#7340=CYLINDRICAL_SURFACE('',#8921,0.225);
#7341=CYLINDRICAL_SURFACE('',#8924,0.225);
#7342=CYLINDRICAL_SURFACE('',#8927,0.225);
#7343=CYLINDRICAL_SURFACE('',#8930,0.62);
#7344=CYLINDRICAL_SURFACE('',#8933,2.);
#7345=CYLINDRICAL_SURFACE('',#8939,0.225);
#7346=CYLINDRICAL_SURFACE('',#8942,0.225);
#7347=CYLINDRICAL_SURFACE('',#8945,0.225);
#7348=CYLINDRICAL_SURFACE('',#8948,0.225);
#7349=CYLINDRICAL_SURFACE('',#8951,0.62);
#7350=CYLINDRICAL_SURFACE('',#8954,2.);
#7351=CYLINDRICAL_SURFACE('',#8960,0.225);
#7352=CYLINDRICAL_SURFACE('',#8963,0.225);
#7353=CYLINDRICAL_SURFACE('',#8966,0.225);
#7354=CYLINDRICAL_SURFACE('',#8969,0.225);
#7355=CYLINDRICAL_SURFACE('',#8972,0.62);
#7356=CYLINDRICAL_SURFACE('',#8975,2.);
#7357=CYLINDRICAL_SURFACE('',#8992,1.05);
#7358=CYLINDRICAL_SURFACE('',#8996,1.);
#7359=CYLINDRICAL_SURFACE('',#9000,1.05);
#7360=CYLINDRICAL_SURFACE('',#9004,1.);
#7361=CYLINDRICAL_SURFACE('',#9008,1.05);
#7362=CYLINDRICAL_SURFACE('',#9012,0.9);
#7363=CYLINDRICAL_SURFACE('',#9025,0.895);
#7364=CYLINDRICAL_SURFACE('',#9029,0.605);
#7365=CYLINDRICAL_SURFACE('',#9047,0.35);
#7366=CYLINDRICAL_SURFACE('',#9055,0.1954);
#7367=CYLINDRICAL_SURFACE('',#9068,0.25);
#7368=CYLINDRICAL_SURFACE('',#9075,0.425);
#7369=CYLINDRICAL_SURFACE('',#9083,0.24505);
#7370=CYLINDRICAL_SURFACE('',#9156,0.4);
#7371=CYLINDRICAL_SURFACE('',#9161,0.9);
#7372=CYLINDRICAL_SURFACE('',#9168,0.99);
#7373=CYLINDRICAL_SURFACE('',#9170,0.225);
#7374=CYLINDRICAL_SURFACE('',#9172,0.99);
#7375=CYLINDRICAL_SURFACE('',#9181,0.165);
#7376=CYLINDRICAL_SURFACE('',#9185,0.4);
#7377=CYLINDRICAL_SURFACE('',#9195,0.35);
#7378=CYLINDRICAL_SURFACE('',#9203,0.1954);
#7379=CYLINDRICAL_SURFACE('',#9217,0.305);
#7380=CYLINDRICAL_SURFACE('',#9220,0.305);
#7381=CYLINDRICAL_SURFACE('',#9225,0.165);
#7382=CYLINDRICAL_SURFACE('',#9230,0.4);
#7383=CYLINDRICAL_SURFACE('',#9255,0.1954);
#7384=CYLINDRICAL_SURFACE('',#9261,0.08);
#7385=CYLINDRICAL_SURFACE('',#9266,0.5);
#7386=CYLINDRICAL_SURFACE('',#9270,0.3);
#7387=CYLINDRICAL_SURFACE('',#9276,0.32);
#7388=CYLINDRICAL_SURFACE('',#9279,0.6);
#7389=CYLINDRICAL_SURFACE('',#9291,0.08);
#7390=CYLINDRICAL_SURFACE('',#9296,0.3);
#7391=CYLINDRICAL_SURFACE('',#9300,0.6);
#7392=CYLINDRICAL_SURFACE('',#9306,0.3);
#7393=CYLINDRICAL_SURFACE('',#9310,0.6);
#7394=CYLINDRICAL_SURFACE('',#9316,0.325);
#7395=CYLINDRICAL_SURFACE('',#9319,0.325);
#7396=CYLINDRICAL_SURFACE('',#9322,0.31);
#7397=CYLINDRICAL_SURFACE('',#9337,0.32);
#7398=CYLINDRICAL_SURFACE('',#9340,0.6);
#7399=CYLINDRICAL_SURFACE('',#9353,0.25175);
#7400=ADVANCED_FACE('',(#1118),#7236,.F.);
#7401=ADVANCED_FACE('',(#1119),#839,.F.);
#7402=ADVANCED_FACE('',(#1120),#7237,.F.);
#7403=ADVANCED_FACE('',(#1121),#840,.F.);
#7404=ADVANCED_FACE('',(#1122),#841,.T.);
#7405=ADVANCED_FACE('',(#1123),#842,.T.);
#7406=ADVANCED_FACE('',(#1124),#7238,.F.);
#7407=ADVANCED_FACE('',(#1125),#7239,.F.);
#7408=ADVANCED_FACE('',(#1126),#7240,.F.);
#7409=ADVANCED_FACE('',(#1127),#843,.F.);
#7410=ADVANCED_FACE('',(#1128),#844,.T.);
#7411=ADVANCED_FACE('',(#1129),#845,.T.);
#7412=ADVANCED_FACE('',(#1130),#846,.T.);
#7413=ADVANCED_FACE('',(#1131),#7241,.F.);
#7414=ADVANCED_FACE('',(#1132),#7242,.F.);
#7415=ADVANCED_FACE('',(#1133),#7243,.F.);
#7416=ADVANCED_FACE('',(#1134),#7244,.F.);
#7417=ADVANCED_FACE('',(#1135),#847,.T.);
#7418=ADVANCED_FACE('',(#1136),#7245,.F.);
#7419=ADVANCED_FACE('',(#1137,#615),#848,.T.);
#7420=ADVANCED_FACE('',(#1138),#7246,.F.);
#7421=ADVANCED_FACE('',(#1139),#7247,.F.);
#7422=ADVANCED_FACE('',(#1140),#7248,.F.);
#7423=ADVANCED_FACE('',(#1141),#7249,.F.);
#7424=ADVANCED_FACE('',(#1142),#7250,.F.);
#7425=ADVANCED_FACE('',(#1143,#616),#849,.T.);
#7426=ADVANCED_FACE('',(#1144,#617,#618,#619,#620,#621),#850,.T.);
#7427=ADVANCED_FACE('',(#1145),#851,.T.);
#7428=ADVANCED_FACE('',(#1146,#622,#623,#624,#625,#626),#852,.T.);
#7429=ADVANCED_FACE('',(#1147),#853,.T.);
#7430=ADVANCED_FACE('',(#1148,#627),#854,.T.);
#7431=ADVANCED_FACE('',(#1149,#628,#629),#855,.F.);
#7432=ADVANCED_FACE('',(#1150),#7251,.F.);
#7433=ADVANCED_FACE('',(#1151,#630),#856,.T.);
#7434=ADVANCED_FACE('',(#1152,#631),#857,.F.);
#7435=ADVANCED_FACE('',(#1153),#7252,.F.);
#7436=ADVANCED_FACE('',(#1154),#7253,.F.);
#7437=ADVANCED_FACE('',(#1155,#632),#858,.F.);
#7438=ADVANCED_FACE('',(#1156,#633),#859,.T.);
#7439=ADVANCED_FACE('',(#1157),#7254,.F.);
#7440=ADVANCED_FACE('',(#1158),#7255,.F.);
#7441=ADVANCED_FACE('',(#1159,#634),#860,.T.);
#7442=ADVANCED_FACE('',(#1160),#861,.F.);
#7443=ADVANCED_FACE('',(#1161),#862,.T.);
#7444=ADVANCED_FACE('',(#1162,#635),#863,.T.);
#7445=ADVANCED_FACE('',(#1163),#864,.T.);
#7446=ADVANCED_FACE('',(#1164),#865,.T.);
#7447=ADVANCED_FACE('',(#1165,#636),#866,.T.);
#7448=ADVANCED_FACE('',(#1166),#867,.F.);
#7449=ADVANCED_FACE('',(#1167),#868,.T.);
#7450=ADVANCED_FACE('',(#1168,#637),#869,.F.);
#7451=ADVANCED_FACE('',(#1169),#870,.T.);
#7452=ADVANCED_FACE('',(#1170),#871,.T.);
#7453=ADVANCED_FACE('',(#1171),#872,.T.);
#7454=ADVANCED_FACE('',(#1172),#873,.T.);
#7455=ADVANCED_FACE('',(#1173),#874,.T.);
#7456=ADVANCED_FACE('',(#1174),#875,.T.);
#7457=ADVANCED_FACE('',(#1175),#876,.T.);
#7458=ADVANCED_FACE('',(#1176),#7256,.F.);
#7459=ADVANCED_FACE('',(#1177),#7257,.T.);
#7460=ADVANCED_FACE('',(#1178,#638),#877,.F.);
#7461=ADVANCED_FACE('',(#1179),#423,.T.);
#7462=ADVANCED_FACE('',(#1180),#424,.T.);
#7463=ADVANCED_FACE('',(#1181),#7258,.T.);
#7464=ADVANCED_FACE('',(#1182,#639),#878,.T.);
#7465=ADVANCED_FACE('',(#1183),#7259,.T.);
#7466=ADVANCED_FACE('',(#1184),#879,.T.);
#7467=ADVANCED_FACE('',(#1185),#7260,.F.);
#7468=ADVANCED_FACE('',(#1186),#880,.F.);
#7469=ADVANCED_FACE('',(#1187),#7261,.F.);
#7470=ADVANCED_FACE('',(#1188),#881,.F.);
#7471=ADVANCED_FACE('',(#1189),#882,.F.);
#7472=ADVANCED_FACE('',(#1190),#883,.F.);
#7473=ADVANCED_FACE('',(#1191),#884,.F.);
#7474=ADVANCED_FACE('',(#1192),#7262,.F.);
#7475=ADVANCED_FACE('',(#1193),#7263,.F.);
#7476=ADVANCED_FACE('',(#1194),#7264,.F.);
#7477=ADVANCED_FACE('',(#1195),#885,.T.);
#7478=ADVANCED_FACE('',(#1196),#886,.T.);
#7479=ADVANCED_FACE('',(#1197),#887,.T.);
#7480=ADVANCED_FACE('',(#1198),#888,.T.);
#7481=ADVANCED_FACE('',(#1199),#7265,.F.);
#7482=ADVANCED_FACE('',(#1200),#7266,.F.);
#7483=ADVANCED_FACE('',(#1201),#7267,.F.);
#7484=ADVANCED_FACE('',(#1202),#889,.F.);
#7485=ADVANCED_FACE('',(#1203),#7268,.F.);
#7486=ADVANCED_FACE('',(#1204,#640),#890,.T.);
#7487=ADVANCED_FACE('',(#1205),#7269,.F.);
#7488=ADVANCED_FACE('',(#1206),#7270,.F.);
#7489=ADVANCED_FACE('',(#1207),#7271,.F.);
#7490=ADVANCED_FACE('',(#1208),#7272,.F.);
#7491=ADVANCED_FACE('',(#1209),#7273,.F.);
#7492=ADVANCED_FACE('',(#1210,#641,#642,#643,#644),#891,.T.);
#7493=ADVANCED_FACE('',(#1211),#892,.T.);
#7494=ADVANCED_FACE('',(#1212,#645,#646,#647,#648,#649),#893,.T.);
#7495=ADVANCED_FACE('',(#1213),#894,.T.);
#7496=ADVANCED_FACE('',(#1214,#650),#895,.T.);
#7497=ADVANCED_FACE('',(#1215,#651,#652),#896,.F.);
#7498=ADVANCED_FACE('',(#1216),#7274,.F.);
#7499=ADVANCED_FACE('',(#1217,#653),#897,.T.);
#7500=ADVANCED_FACE('',(#1218,#654),#898,.F.);
#7501=ADVANCED_FACE('',(#1219),#7275,.F.);
#7502=ADVANCED_FACE('',(#1220),#7276,.F.);
#7503=ADVANCED_FACE('',(#1221,#655),#899,.F.);
#7504=ADVANCED_FACE('',(#1222,#656),#900,.T.);
#7505=ADVANCED_FACE('',(#1223),#7277,.F.);
#7506=ADVANCED_FACE('',(#1224),#7278,.F.);
#7507=ADVANCED_FACE('',(#1225,#657),#901,.T.);
#7508=ADVANCED_FACE('',(#1226),#902,.F.);
#7509=ADVANCED_FACE('',(#1227),#903,.T.);
#7510=ADVANCED_FACE('',(#1228,#658),#904,.T.);
#7511=ADVANCED_FACE('',(#1229),#905,.T.);
#7512=ADVANCED_FACE('',(#1230),#906,.T.);
#7513=ADVANCED_FACE('',(#1231,#659),#907,.T.);
#7514=ADVANCED_FACE('',(#1232),#908,.F.);
#7515=ADVANCED_FACE('',(#1233),#909,.T.);
#7516=ADVANCED_FACE('',(#1234,#660),#910,.F.);
#7517=ADVANCED_FACE('',(#1235),#911,.T.);
#7518=ADVANCED_FACE('',(#1236),#912,.T.);
#7519=ADVANCED_FACE('',(#1237),#913,.T.);
#7520=ADVANCED_FACE('',(#1238),#914,.T.);
#7521=ADVANCED_FACE('',(#1239),#915,.T.);
#7522=ADVANCED_FACE('',(#1240),#916,.T.);
#7523=ADVANCED_FACE('',(#1241),#917,.T.);
#7524=ADVANCED_FACE('',(#1242),#7279,.F.);
#7525=ADVANCED_FACE('',(#1243),#7280,.T.);
#7526=ADVANCED_FACE('',(#1244,#661),#918,.F.);
#7527=ADVANCED_FACE('',(#1245),#425,.T.);
#7528=ADVANCED_FACE('',(#1246),#426,.T.);
#7529=ADVANCED_FACE('',(#1247),#7281,.T.);
#7530=ADVANCED_FACE('',(#1248,#662),#919,.T.);
#7531=ADVANCED_FACE('',(#1249),#7282,.T.);
#7532=ADVANCED_FACE('',(#1250),#920,.T.);
#7533=ADVANCED_FACE('',(#1251),#7283,.F.);
#7534=ADVANCED_FACE('',(#1252),#7284,.T.);
#7535=ADVANCED_FACE('',(#1253,#663),#921,.T.);
#7536=ADVANCED_FACE('',(#1254,#664),#922,.F.);
#7537=ADVANCED_FACE('',(#1255),#7285,.F.);
#7538=ADVANCED_FACE('',(#1256),#7286,.T.);
#7539=ADVANCED_FACE('',(#1257,#665),#923,.T.);
#7540=ADVANCED_FACE('',(#1258,#666),#924,.F.);
#7541=ADVANCED_FACE('',(#1259),#7287,.F.);
#7542=ADVANCED_FACE('',(#1260),#7288,.T.);
#7543=ADVANCED_FACE('',(#1261,#667),#925,.T.);
#7544=ADVANCED_FACE('',(#1262,#668),#926,.F.);
#7545=ADVANCED_FACE('',(#1263),#7289,.F.);
#7546=ADVANCED_FACE('',(#1264,#669),#927,.T.);
#7547=ADVANCED_FACE('',(#1265),#7290,.F.);
#7548=ADVANCED_FACE('',(#1266,#670),#928,.T.);
#7549=ADVANCED_FACE('',(#1267),#7291,.F.);
#7550=ADVANCED_FACE('',(#1268),#7292,.F.);
#7551=ADVANCED_FACE('',(#1269),#7293,.F.);
#7552=ADVANCED_FACE('',(#1270,#671),#929,.F.);
#7553=ADVANCED_FACE('',(#1271),#7294,.F.);
#7554=ADVANCED_FACE('',(#1272,#672),#930,.F.);
#7555=ADVANCED_FACE('',(#1273),#7295,.F.);
#7556=ADVANCED_FACE('',(#1274),#7296,.F.);
#7557=ADVANCED_FACE('',(#1275),#931,.T.);
#7558=ADVANCED_FACE('',(#1276),#932,.T.);
#7559=ADVANCED_FACE('',(#1277),#933,.T.);
#7560=ADVANCED_FACE('',(#1278),#934,.T.);
#7561=ADVANCED_FACE('',(#1279,#673,#674,#675,#676),#935,.T.);
#7562=ADVANCED_FACE('',(#1280,#677,#678,#679,#680),#936,.F.);
#7563=ADVANCED_FACE('',(#1281),#937,.T.);
#7564=ADVANCED_FACE('',(#1282),#427,.T.);
#7565=ADVANCED_FACE('',(#1283),#7297,.T.);
#7566=ADVANCED_FACE('',(#1284),#428,.T.);
#7567=ADVANCED_FACE('',(#1285,#681),#938,.T.);
#7568=ADVANCED_FACE('',(#1286),#429,.T.);
#7569=ADVANCED_FACE('',(#1287),#7298,.T.);
#7570=ADVANCED_FACE('',(#1288),#430,.T.);
#7571=ADVANCED_FACE('',(#1289),#939,.T.);
#7572=ADVANCED_FACE('',(#1290),#940,.F.);
#7573=ADVANCED_FACE('',(#1291),#941,.F.);
#7574=ADVANCED_FACE('',(#1292),#942,.F.);
#7575=ADVANCED_FACE('',(#1293),#943,.F.);
#7576=ADVANCED_FACE('',(#1294),#944,.F.);
#7577=ADVANCED_FACE('',(#1295),#945,.F.);
#7578=ADVANCED_FACE('',(#1296),#946,.F.);
#7579=ADVANCED_FACE('',(#1297),#947,.F.);
#7580=ADVANCED_FACE('',(#1298),#7299,.F.);
#7581=ADVANCED_FACE('',(#1299,#682),#948,.T.);
#7582=ADVANCED_FACE('',(#1300,#683),#949,.T.);
#7583=ADVANCED_FACE('',(#1301,#684),#950,.F.);
#7584=ADVANCED_FACE('',(#1302),#951,.T.);
#7585=ADVANCED_FACE('',(#1303),#952,.T.);
#7586=ADVANCED_FACE('',(#1304),#953,.T.);
#7587=ADVANCED_FACE('',(#1305),#954,.T.);
#7588=ADVANCED_FACE('',(#1306),#955,.T.);
#7589=ADVANCED_FACE('',(#1307),#956,.T.);
#7590=ADVANCED_FACE('',(#1308,#685),#957,.T.);
#7591=ADVANCED_FACE('',(#1309),#7300,.F.);
#7592=ADVANCED_FACE('',(#1310,#686),#958,.T.);
#7593=ADVANCED_FACE('',(#1311),#7301,.T.);
#7594=ADVANCED_FACE('',(#1312),#7302,.T.);
#7595=ADVANCED_FACE('',(#1313,#687),#959,.T.);
#7596=ADVANCED_FACE('',(#1314),#7303,.F.);
#7597=ADVANCED_FACE('',(#1315,#688),#960,.T.);
#7598=ADVANCED_FACE('',(#1316),#7304,.T.);
#7599=ADVANCED_FACE('',(#1317,#689),#961,.T.);
#7600=ADVANCED_FACE('',(#1318),#7305,.T.);
#7601=ADVANCED_FACE('',(#1319,#690),#962,.T.);
#7602=ADVANCED_FACE('',(#1320),#7306,.F.);
#7603=ADVANCED_FACE('',(#1321),#43,.T.);
#7604=ADVANCED_FACE('',(#1322),#7307,.F.);
#7605=ADVANCED_FACE('',(#1323,#691),#963,.F.);
#7606=ADVANCED_FACE('',(#1324,#692),#964,.T.);
#7607=ADVANCED_FACE('',(#1325),#7308,.F.);
#7608=ADVANCED_FACE('',(#1326),#7309,.F.);
#7609=ADVANCED_FACE('',(#1327),#7310,.T.);
#7610=ADVANCED_FACE('',(#1328,#693),#965,.T.);
#7611=ADVANCED_FACE('',(#1329,#694),#966,.F.);
#7612=ADVANCED_FACE('',(#1330),#44,.T.);
#7613=ADVANCED_FACE('',(#1331),#7311,.T.);
#7614=ADVANCED_FACE('',(#1332),#967,.T.);
#7615=ADVANCED_FACE('',(#1333),#968,.F.);
#7616=ADVANCED_FACE('',(#1334),#431,.F.);
#7617=ADVANCED_FACE('',(#1335),#7312,.F.);
#7618=ADVANCED_FACE('',(#1336,#695),#969,.T.);
#7619=ADVANCED_FACE('',(#1337),#7313,.T.);
#7620=ADVANCED_FACE('',(#1338,#696),#970,.F.);
#7621=ADVANCED_FACE('',(#1339),#432,.T.);
#7622=ADVANCED_FACE('',(#1340),#433,.T.);
#7623=ADVANCED_FACE('',(#1341),#971,.T.);
#7624=ADVANCED_FACE('',(#1342),#972,.T.);
#7625=ADVANCED_FACE('',(#1343),#973,.T.);
#7626=ADVANCED_FACE('',(#1344),#7314,.F.);
#7627=ADVANCED_FACE('',(#1345),#974,.T.);
#7628=ADVANCED_FACE('',(#1346),#975,.T.);
#7629=ADVANCED_FACE('',(#1347),#976,.T.);
#7630=ADVANCED_FACE('',(#1348,#697),#977,.T.);
#7631=ADVANCED_FACE('',(#1349,#698),#978,.F.);
#7632=ADVANCED_FACE('',(#1350),#7315,.F.);
#7633=ADVANCED_FACE('',(#1351),#7316,.F.);
#7634=ADVANCED_FACE('',(#1352),#7317,.F.);
#7635=ADVANCED_FACE('',(#1353),#7318,.F.);
#7636=ADVANCED_FACE('',(#1354),#7319,.F.);
#7637=ADVANCED_FACE('',(#1355),#7320,.F.);
#7638=ADVANCED_FACE('',(#1356),#7321,.F.);
#7639=ADVANCED_FACE('',(#1357),#7322,.F.);
#7640=ADVANCED_FACE('',(#1358),#7323,.F.);
#7641=ADVANCED_FACE('',(#1359),#7324,.F.);
#7642=ADVANCED_FACE('',(#1360),#7325,.F.);
#7643=ADVANCED_FACE('',(#1361),#7326,.F.);
#7644=ADVANCED_FACE('',(#1362),#7327,.F.);
#7645=ADVANCED_FACE('',(#1363),#979,.T.);
#7646=ADVANCED_FACE('',(#1364),#980,.T.);
#7647=ADVANCED_FACE('',(#1365),#981,.T.);
#7648=ADVANCED_FACE('',(#1366,#699,#700,#701,#702,#703),#982,.T.);
#7649=ADVANCED_FACE('',(#1367,#704,#705,#706,#707,#708),#983,.F.);
#7650=ADVANCED_FACE('',(#1368),#7328,.F.);
#7651=ADVANCED_FACE('',(#1369),#7329,.F.);
#7652=ADVANCED_FACE('',(#1370),#7330,.F.);
#7653=ADVANCED_FACE('',(#1371),#7331,.F.);
#7654=ADVANCED_FACE('',(#1372),#7332,.F.);
#7655=ADVANCED_FACE('',(#1373),#984,.T.);
#7656=ADVANCED_FACE('',(#1374),#985,.T.);
#7657=ADVANCED_FACE('',(#1375),#986,.T.);
#7658=ADVANCED_FACE('',(#1376,#709,#710,#711,#712,#713),#987,.T.);
#7659=ADVANCED_FACE('',(#1377,#714,#715,#716,#717,#718),#988,.F.);
#7660=ADVANCED_FACE('',(#1378),#989,.T.);
#7661=ADVANCED_FACE('',(#1379),#990,.T.);
#7662=ADVANCED_FACE('',(#1380),#991,.T.);
#7663=ADVANCED_FACE('',(#1381),#992,.T.);
#7664=ADVANCED_FACE('',(#1382,#719,#720,#721,#722,#723,#724,#725,#726,#727,
#728),#993,.T.);
#7665=ADVANCED_FACE('',(#1383,#729,#730,#731,#732,#733,#734,#735,#736),
#994,.F.);
#7666=ADVANCED_FACE('',(#1384),#7333,.F.);
#7667=ADVANCED_FACE('',(#1385),#7334,.F.);
#7668=ADVANCED_FACE('',(#1386),#7335,.F.);
#7669=ADVANCED_FACE('',(#1387),#7336,.F.);
#7670=ADVANCED_FACE('',(#1388),#7337,.F.);
#7671=ADVANCED_FACE('',(#1389),#7338,.T.);
#7672=ADVANCED_FACE('',(#1390,#737,#738,#739,#740,#741),#995,.T.);
#7673=ADVANCED_FACE('',(#1391,#742,#743,#744,#745,#746),#996,.F.);
#7674=ADVANCED_FACE('',(#1392),#7339,.F.);
#7675=ADVANCED_FACE('',(#1393),#7340,.F.);
#7676=ADVANCED_FACE('',(#1394),#7341,.F.);
#7677=ADVANCED_FACE('',(#1395),#7342,.F.);
#7678=ADVANCED_FACE('',(#1396),#7343,.F.);
#7679=ADVANCED_FACE('',(#1397),#7344,.T.);
#7680=ADVANCED_FACE('',(#1398,#747,#748,#749,#750,#751),#997,.T.);
#7681=ADVANCED_FACE('',(#1399,#752,#753,#754,#755,#756),#998,.F.);
#7682=ADVANCED_FACE('',(#1400),#7345,.F.);
#7683=ADVANCED_FACE('',(#1401),#7346,.F.);
#7684=ADVANCED_FACE('',(#1402),#7347,.F.);
#7685=ADVANCED_FACE('',(#1403),#7348,.F.);
#7686=ADVANCED_FACE('',(#1404),#7349,.F.);
#7687=ADVANCED_FACE('',(#1405),#7350,.T.);
#7688=ADVANCED_FACE('',(#1406,#757,#758,#759,#760,#761),#999,.T.);
#7689=ADVANCED_FACE('',(#1407,#762,#763,#764,#765,#766),#1000,.F.);
#7690=ADVANCED_FACE('',(#1408),#7351,.F.);
#7691=ADVANCED_FACE('',(#1409),#7352,.F.);
#7692=ADVANCED_FACE('',(#1410),#7353,.F.);
#7693=ADVANCED_FACE('',(#1411),#7354,.F.);
#7694=ADVANCED_FACE('',(#1412),#7355,.F.);
#7695=ADVANCED_FACE('',(#1413),#7356,.T.);
#7696=ADVANCED_FACE('',(#1414,#767,#768,#769,#770,#771),#1001,.T.);
#7697=ADVANCED_FACE('',(#1415,#772,#773,#774,#775,#776),#1002,.F.);
#7698=ADVANCED_FACE('',(#1416),#1003,.F.);
#7699=ADVANCED_FACE('',(#1417),#1004,.F.);
#7700=ADVANCED_FACE('',(#1418),#1005,.F.);
#7701=ADVANCED_FACE('',(#1419),#1006,.F.);
#7702=ADVANCED_FACE('',(#1420),#1007,.F.);
#7703=ADVANCED_FACE('',(#1421,#777),#1008,.T.);
#7704=ADVANCED_FACE('',(#1422),#7357,.T.);
#7705=ADVANCED_FACE('',(#1423,#778),#1009,.T.);
#7706=ADVANCED_FACE('',(#1424),#7358,.T.);
#7707=ADVANCED_FACE('',(#1425,#779),#1010,.T.);
#7708=ADVANCED_FACE('',(#1426),#7359,.T.);
#7709=ADVANCED_FACE('',(#1427,#780),#1011,.T.);
#7710=ADVANCED_FACE('',(#1428),#7360,.T.);
#7711=ADVANCED_FACE('',(#1429,#781),#1012,.T.);
#7712=ADVANCED_FACE('',(#1430),#7361,.T.);
#7713=ADVANCED_FACE('',(#1431,#782),#1013,.T.);
#7714=ADVANCED_FACE('',(#1432,#783),#7362,.F.);
#7715=ADVANCED_FACE('',(#1433),#1014,.F.);
#7716=ADVANCED_FACE('',(#1434),#1015,.F.);
#7717=ADVANCED_FACE('',(#1435),#1016,.F.);
#7718=ADVANCED_FACE('',(#1436),#1017,.F.);
#7719=ADVANCED_FACE('',(#1437,#784),#1018,.T.);
#7720=ADVANCED_FACE('',(#1438,#785),#7363,.T.);
#7721=ADVANCED_FACE('',(#1439,#786),#1019,.T.);
#7722=ADVANCED_FACE('',(#1440,#787),#7364,.F.);
#7723=ADVANCED_FACE('',(#1441),#1020,.F.);
#7724=ADVANCED_FACE('',(#1442),#1021,.F.);
#7725=ADVANCED_FACE('',(#1443),#1022,.F.);
#7726=ADVANCED_FACE('',(#1444),#1023,.F.);
#7727=ADVANCED_FACE('',(#1445),#1024,.F.);
#7728=ADVANCED_FACE('',(#1446),#1025,.F.);
#7729=ADVANCED_FACE('',(#1447),#1026,.F.);
#7730=ADVANCED_FACE('',(#1448),#1027,.F.);
#7731=ADVANCED_FACE('',(#1449),#1028,.F.);
#7732=ADVANCED_FACE('',(#1450),#1029,.T.);
#7733=ADVANCED_FACE('',(#1451),#434,.T.);
#7734=ADVANCED_FACE('',(#1452),#7365,.T.);
#7735=ADVANCED_FACE('',(#1453),#435,.T.);
#7736=ADVANCED_FACE('',(#1454,#788),#1030,.T.);
#7737=ADVANCED_FACE('',(#1455),#436,.T.);
#7738=ADVANCED_FACE('',(#1456),#7366,.T.);
#7739=ADVANCED_FACE('',(#1457),#1031,.F.);
#7740=ADVANCED_FACE('',(#1458),#1032,.F.);
#7741=ADVANCED_FACE('',(#1459),#1033,.F.);
#7742=ADVANCED_FACE('',(#1460),#1034,.F.);
#7743=ADVANCED_FACE('',(#1461),#1035,.F.);
#7744=ADVANCED_FACE('',(#1462),#1036,.F.);
#7745=ADVANCED_FACE('',(#1463),#1037,.F.);
#7746=ADVANCED_FACE('',(#1464),#1038,.F.);
#7747=ADVANCED_FACE('',(#1465,#789),#1039,.T.);
#7748=ADVANCED_FACE('',(#1466),#7367,.T.);
#7749=ADVANCED_FACE('',(#1467),#1040,.F.);
#7750=ADVANCED_FACE('',(#1468),#1041,.T.);
#7751=ADVANCED_FACE('',(#1469),#437,.T.);
#7752=ADVANCED_FACE('',(#1470),#7368,.T.);
#7753=ADVANCED_FACE('',(#1471),#438,.T.);
#7754=ADVANCED_FACE('',(#1472,#790),#1042,.T.);
#7755=ADVANCED_FACE('',(#1473),#439,.T.);
#7756=ADVANCED_FACE('',(#1474),#7369,.T.);
#7757=ADVANCED_FACE('',(#1475),#440,.T.);
#7758=ADVANCED_FACE('',(#1476),#7370,.F.);
#7759=ADVANCED_FACE('',(#1477,#791),#1043,.T.);
#7760=ADVANCED_FACE('',(#1478),#7371,.T.);
#7761=ADVANCED_FACE('',(#1479,#792),#1044,.F.);
#7762=ADVANCED_FACE('',(#1480,#793),#1045,.T.);
#7763=ADVANCED_FACE('',(#1481),#7372,.T.);
#7764=ADVANCED_FACE('',(#1482),#7373,.F.);
#7765=ADVANCED_FACE('',(#1483),#7374,.T.);
#7766=ADVANCED_FACE('',(#1484,#794),#1046,.T.);
#7767=ADVANCED_FACE('',(#1485,#795),#1047,.F.);
#7768=ADVANCED_FACE('',(#1486),#45,.T.);
#7769=ADVANCED_FACE('',(#1487),#7375,.F.);
#7770=ADVANCED_FACE('',(#1488),#1048,.T.);
#7771=ADVANCED_FACE('',(#1489),#7376,.T.);
#7772=ADVANCED_FACE('',(#1490,#796),#1049,.T.);
#7773=ADVANCED_FACE('',(#1491),#1050,.F.);
#7774=ADVANCED_FACE('',(#1492),#1051,.T.);
#7775=ADVANCED_FACE('',(#1493),#441,.T.);
#7776=ADVANCED_FACE('',(#1494),#7377,.T.);
#7777=ADVANCED_FACE('',(#1495),#442,.T.);
#7778=ADVANCED_FACE('',(#1496,#797),#1052,.T.);
#7779=ADVANCED_FACE('',(#1497),#443,.T.);
#7780=ADVANCED_FACE('',(#1498),#7378,.T.);
#7781=ADVANCED_FACE('',(#1499),#444,.T.);
#7782=ADVANCED_FACE('',(#1500),#1053,.T.);
#7783=ADVANCED_FACE('',(#1501),#1054,.F.);
#7784=ADVANCED_FACE('',(#1502),#1055,.F.);
#7785=ADVANCED_FACE('',(#1503),#1056,.F.);
#7786=ADVANCED_FACE('',(#1504),#1057,.F.);
#7787=ADVANCED_FACE('',(#1505),#1058,.F.);
#7788=ADVANCED_FACE('',(#1506),#1059,.F.);
#7789=ADVANCED_FACE('',(#1507),#1060,.F.);
#7790=ADVANCED_FACE('',(#1508),#1061,.F.);
#7791=ADVANCED_FACE('',(#1509),#7379,.F.);
#7792=ADVANCED_FACE('',(#1510),#7380,.F.);
#7793=ADVANCED_FACE('',(#1511),#1062,.T.);
#7794=ADVANCED_FACE('',(#1512),#7381,.F.);
#7795=ADVANCED_FACE('',(#1513),#1063,.T.);
#7796=ADVANCED_FACE('',(#1514,#798),#7382,.F.);
#7797=ADVANCED_FACE('',(#1515,#799),#1064,.F.);
#7798=ADVANCED_FACE('',(#1516,#800),#1065,.F.);
#7799=ADVANCED_FACE('',(#1517,#801),#1066,.F.);
#7800=ADVANCED_FACE('',(#1518),#1067,.F.);
#7801=ADVANCED_FACE('',(#1519),#1068,.T.);
#7802=ADVANCED_FACE('',(#1520),#1069,.T.);
#7803=ADVANCED_FACE('',(#1521,#802),#1070,.T.);
#7804=ADVANCED_FACE('',(#1522,#803),#1071,.T.);
#7805=ADVANCED_FACE('',(#1523,#804),#1072,.T.);
#7806=ADVANCED_FACE('',(#1524,#805),#1073,.T.);
#7807=ADVANCED_FACE('',(#1525),#1074,.F.);
#7808=ADVANCED_FACE('',(#1526),#1075,.F.);
#7809=ADVANCED_FACE('',(#1527),#1076,.F.);
#7810=ADVANCED_FACE('',(#1528),#1077,.F.);
#7811=ADVANCED_FACE('',(#1529),#1078,.F.);
#7812=ADVANCED_FACE('',(#1530),#1079,.F.);
#7813=ADVANCED_FACE('',(#1531),#1080,.F.);
#7814=ADVANCED_FACE('',(#1532,#806),#1081,.T.);
#7815=ADVANCED_FACE('',(#1533),#445,.T.);
#7816=ADVANCED_FACE('',(#1534),#7383,.T.);
#7817=ADVANCED_FACE('',(#1535),#446,.T.);
#7818=ADVANCED_FACE('',(#1536),#1082,.T.);
#7819=ADVANCED_FACE('',(#1537),#7384,.F.);
#7820=ADVANCED_FACE('',(#1538),#1083,.T.);
#7821=ADVANCED_FACE('',(#1539),#447,.T.);
#7822=ADVANCED_FACE('',(#1540),#7385,.T.);
#7823=ADVANCED_FACE('',(#1541,#807),#1084,.T.);
#7824=ADVANCED_FACE('',(#1542,#808),#7386,.T.);
#7825=ADVANCED_FACE('',(#1543),#448,.T.);
#7826=ADVANCED_FACE('',(#1544),#1085,.T.);
#7827=ADVANCED_FACE('',(#1545),#7387,.F.);
#7828=ADVANCED_FACE('',(#1546),#7388,.T.);
#7829=ADVANCED_FACE('',(#1547,#809),#1086,.T.);
#7830=ADVANCED_FACE('',(#1548,#810),#1087,.F.);
#7831=ADVANCED_FACE('',(#1549,#811),#46,.T.);
#7832=ADVANCED_FACE('',(#1550),#1088,.F.);
#7833=ADVANCED_FACE('',(#1551),#1089,.T.);
#7834=ADVANCED_FACE('',(#1552),#7389,.T.);
#7835=ADVANCED_FACE('',(#1553),#1090,.F.);
#7836=ADVANCED_FACE('',(#1554),#7390,.T.);
#7837=ADVANCED_FACE('',(#1555),#1091,.F.);
#7838=ADVANCED_FACE('',(#1556),#7391,.T.);
#7839=ADVANCED_FACE('',(#1557),#1092,.T.);
#7840=ADVANCED_FACE('',(#1558,#812),#1093,.F.);
#7841=ADVANCED_FACE('',(#1559),#7392,.T.);
#7842=ADVANCED_FACE('',(#1560),#1094,.F.);
#7843=ADVANCED_FACE('',(#1561),#7393,.T.);
#7844=ADVANCED_FACE('',(#1562),#1095,.T.);
#7845=ADVANCED_FACE('',(#1563,#813),#1096,.F.);
#7846=ADVANCED_FACE('',(#1564),#7394,.F.);
#7847=ADVANCED_FACE('',(#1565),#7395,.F.);
#7848=ADVANCED_FACE('',(#1566),#7396,.F.);
#7849=ADVANCED_FACE('',(#1567),#1097,.F.);
#7850=ADVANCED_FACE('',(#1568,#814),#1098,.T.);
#7851=ADVANCED_FACE('',(#1569),#1099,.T.);
#7852=ADVANCED_FACE('',(#1570,#815),#1100,.T.);
#7853=ADVANCED_FACE('',(#1571),#1101,.T.);
#7854=ADVANCED_FACE('',(#1572,#816,#817,#818),#1102,.T.);
#7855=ADVANCED_FACE('',(#1573),#1103,.T.);
#7856=ADVANCED_FACE('',(#1574,#819,#820),#1104,.T.);
#7857=ADVANCED_FACE('',(#1575),#1105,.T.);
#7858=ADVANCED_FACE('',(#1576),#1106,.T.);
#7859=ADVANCED_FACE('',(#1577),#1107,.F.);
#7860=ADVANCED_FACE('',(#1578),#7397,.F.);
#7861=ADVANCED_FACE('',(#1579),#7398,.T.);
#7862=ADVANCED_FACE('',(#1580,#821),#1108,.T.);
#7863=ADVANCED_FACE('',(#1581,#822),#1109,.F.);
#7864=ADVANCED_FACE('',(#1582),#449,.T.);
#7865=ADVANCED_FACE('',(#1583),#450,.T.);
#7866=ADVANCED_FACE('',(#1584),#1110,.T.);
#7867=ADVANCED_FACE('',(#1585),#1111,.T.);
#7868=ADVANCED_FACE('',(#1586),#1112,.T.);
#7869=ADVANCED_FACE('',(#1587),#7399,.F.);
#7870=ADVANCED_FACE('',(#1588),#1113,.T.);
#7871=ADVANCED_FACE('',(#1589),#1114,.T.);
#7872=ADVANCED_FACE('',(#1590),#1115,.T.);
#7873=ADVANCED_FACE('',(#1591,#823),#1116,.T.);
#7874=ADVANCED_FACE('',(#1592,#824),#1117,.F.);
#7875=CLOSED_SHELL('',(#7400,#7401,#7402,#7403,#7404,#7405,#7406,#7407,
#7408,#7409,#7410,#7411,#7412,#7413,#7414,#7415,#7416,#7417,#7418,#7419,
#7420,#7421,#7422,#7423,#7424,#7425,#7426,#7427,#7428,#7429,#7430,#7431));
#7876=CLOSED_SHELL('',(#7432,#7433,#7434,#7435,#7436,#7437,#7438,#7439,
#7440,#7441,#7442,#7443,#7444,#7445,#7446,#7447,#7448,#7449,#7450,#7451,
#7452,#7453,#7454,#7455,#7456,#7457,#7458,#7459,#7460));
#7877=CLOSED_SHELL('',(#7461,#7462,#7463,#7464,#7465,#7466));
#7878=CLOSED_SHELL('',(#7467,#7468,#7469,#7470,#7471,#7472,#7473,#7474,
#7475,#7476,#7477,#7478,#7479,#7480,#7481,#7482,#7483,#7484,#7485,#7486,
#7487,#7488,#7489,#7490,#7491,#7492,#7493,#7494,#7495,#7496,#7497));
#7879=CLOSED_SHELL('',(#7498,#7499,#7500,#7501,#7502,#7503,#7504,#7505,
#7506,#7507,#7508,#7509,#7510,#7511,#7512,#7513,#7514,#7515,#7516,#7517,
#7518,#7519,#7520,#7521,#7522,#7523,#7524,#7525,#7526));
#7880=CLOSED_SHELL('',(#7527,#7528,#7529,#7530,#7531,#7532));
#7881=CLOSED_SHELL('',(#7533,#7534,#7535,#7536));
#7882=CLOSED_SHELL('',(#7537,#7538,#7539,#7540));
#7883=CLOSED_SHELL('',(#7541,#7542,#7543,#7544));
#7884=CLOSED_SHELL('',(#7545,#7546,#7547,#7548,#7549,#7550,#7551,#7552,
#7553,#7554,#7555,#7556,#7557,#7558,#7559,#7560,#7561,#7562));
#7885=CLOSED_SHELL('',(#7563,#7564,#7565,#7566,#7567,#7568,#7569,#7570,
#7571));
#7886=CLOSED_SHELL('',(#7572,#7573,#7574,#7575,#7576,#7577,#7578,#7579));
#7887=CLOSED_SHELL('',(#7580,#7581,#7582,#7583,#7584,#7585,#7586,#7587,
#7588,#7589,#7590,#7591,#7592,#7593,#7594,#7595,#7596));
#7888=CLOSED_SHELL('',(#7597,#7598,#7599,#7600,#7601,#7602));
#7889=CLOSED_SHELL('',(#7603));
#7890=CLOSED_SHELL('',(#7604,#7605,#7606,#7607,#7608,#7609,#7610,#7611));
#7891=CLOSED_SHELL('',(#7612));
#7892=CLOSED_SHELL('',(#7613,#7614,#7615));
#7893=CLOSED_SHELL('',(#7616,#7617,#7618,#7619,#7620));
#7894=CLOSED_SHELL('',(#7621,#7622,#7623,#7624,#7625,#7626,#7627,#7628,
#7629,#7630,#7631));
#7895=CLOSED_SHELL('',(#7632,#7633,#7634,#7635,#7636,#7637,#7638,#7639,
#7640,#7641,#7642,#7643,#7644,#7645,#7646,#7647,#7648,#7649,#7650,#7651,
#7652,#7653,#7654,#7655,#7656,#7657,#7658,#7659,#7660,#7661,#7662,#7663,
#7664,#7665));
#7896=CLOSED_SHELL('',(#7666,#7667,#7668,#7669,#7670,#7671,#7672,#7673));
#7897=CLOSED_SHELL('',(#7674,#7675,#7676,#7677,#7678,#7679,#7680,#7681));
#7898=CLOSED_SHELL('',(#7682,#7683,#7684,#7685,#7686,#7687,#7688,#7689));
#7899=CLOSED_SHELL('',(#7690,#7691,#7692,#7693,#7694,#7695,#7696,#7697));
#7900=CLOSED_SHELL('',(#7698,#7699,#7700,#7701,#7702,#7703,#7704,#7705,
#7706,#7707,#7708,#7709,#7710,#7711,#7712,#7713,#7714));
#7901=CLOSED_SHELL('',(#7715,#7716,#7717,#7718,#7719,#7720,#7721,#7722));
#7902=CLOSED_SHELL('',(#7723,#7724,#7725,#7726,#7727,#7728,#7729,#7730));
#7903=CLOSED_SHELL('',(#7731,#7732,#7733,#7734,#7735,#7736,#7737,#7738));
#7904=CLOSED_SHELL('',(#7739,#7740,#7741,#7742,#7743,#7744,#7745,#7746));
#7905=CLOSED_SHELL('',(#7747,#7748,#7749,#7750,#7751,#7752,#7753,#7754,
#7755,#7756,#7757));
#7906=CLOSED_SHELL('',(#7758,#7759,#7760,#7761,#7762,#7763,#7764,#7765,
#7766,#7767));
#7907=CLOSED_SHELL('',(#7768));
#7908=CLOSED_SHELL('',(#7769,#7770,#7771,#7772,#7773));
#7909=CLOSED_SHELL('',(#7774,#7775,#7776,#7777,#7778,#7779,#7780,#7781,
#7782));
#7910=CLOSED_SHELL('',(#7783,#7784,#7785,#7786,#7787,#7788,#7789,#7790));
#7911=CLOSED_SHELL('',(#7791,#7792,#7793,#7794,#7795,#7796,#7797,#7798,
#7799,#7800,#7801,#7802,#7803,#7804,#7805,#7806));
#7912=CLOSED_SHELL('',(#7807,#7808,#7809,#7810,#7811,#7812,#7813,#7814,
#7815,#7816,#7817,#7818));
#7913=CLOSED_SHELL('',(#7819,#7820,#7821,#7822,#7823,#7824,#7825,#7826));
#7914=CLOSED_SHELL('',(#7827,#7828,#7829,#7830));
#7915=CLOSED_SHELL('',(#7831,#7832,#7833,#7834,#7835));
#7916=CLOSED_SHELL('',(#7836,#7837,#7838,#7839,#7840));
#7917=CLOSED_SHELL('',(#7841,#7842,#7843,#7844,#7845));
#7918=CLOSED_SHELL('',(#7846,#7847,#7848,#7849,#7850,#7851,#7852,#7853,
#7854,#7855,#7856,#7857,#7858,#7859));
#7919=CLOSED_SHELL('',(#7860,#7861,#7862,#7863));
#7920=CLOSED_SHELL('',(#7864,#7865,#7866,#7867,#7868,#7869,#7870,#7871,
#7872,#7873,#7874));
#7921=DERIVED_UNIT_ELEMENT(#8005,1.);
#7922=DERIVED_UNIT_ELEMENT(#14394,-3.);
#7923=DERIVED_UNIT_ELEMENT(#8005,1.);
#7924=DERIVED_UNIT_ELEMENT(#14394,-3.);
#7925=DERIVED_UNIT_ELEMENT(#8005,1.);
#7926=DERIVED_UNIT_ELEMENT(#14394,-3.);
#7927=DERIVED_UNIT_ELEMENT(#8005,1.);
#7928=DERIVED_UNIT_ELEMENT(#14394,-3.);
#7929=DERIVED_UNIT_ELEMENT(#8005,1.);
#7930=DERIVED_UNIT_ELEMENT(#14394,-3.);
#7931=DERIVED_UNIT_ELEMENT(#8005,1.);
#7932=DERIVED_UNIT_ELEMENT(#14394,-3.);
#7933=DERIVED_UNIT_ELEMENT(#8005,1.);
#7934=DERIVED_UNIT_ELEMENT(#14394,-3.);
#7935=DERIVED_UNIT_ELEMENT(#8005,1.);
#7936=DERIVED_UNIT_ELEMENT(#14394,-3.);
#7937=DERIVED_UNIT_ELEMENT(#8005,1.);
#7938=DERIVED_UNIT_ELEMENT(#14394,-3.);
#7939=DERIVED_UNIT_ELEMENT(#8005,1.);
#7940=DERIVED_UNIT_ELEMENT(#14394,-3.);
#7941=DERIVED_UNIT_ELEMENT(#8005,1.);
#7942=DERIVED_UNIT_ELEMENT(#14394,-3.);
#7943=DERIVED_UNIT_ELEMENT(#8005,1.);
#7944=DERIVED_UNIT_ELEMENT(#14394,-3.);
#7945=DERIVED_UNIT_ELEMENT(#8005,1.);
#7946=DERIVED_UNIT_ELEMENT(#14394,-3.);
#7947=DERIVED_UNIT_ELEMENT(#8005,1.);
#7948=DERIVED_UNIT_ELEMENT(#14394,-3.);
#7949=DERIVED_UNIT_ELEMENT(#8005,1.);
#7950=DERIVED_UNIT_ELEMENT(#14394,-3.);
#7951=DERIVED_UNIT_ELEMENT(#8005,1.);
#7952=DERIVED_UNIT_ELEMENT(#14394,-3.);
#7953=DERIVED_UNIT_ELEMENT(#8005,1.);
#7954=DERIVED_UNIT_ELEMENT(#14394,-3.);
#7955=DERIVED_UNIT_ELEMENT(#8005,1.);
#7956=DERIVED_UNIT_ELEMENT(#14394,-3.);
#7957=DERIVED_UNIT_ELEMENT(#8005,1.);
#7958=DERIVED_UNIT_ELEMENT(#14394,-3.);
#7959=DERIVED_UNIT_ELEMENT(#8005,1.);
#7960=DERIVED_UNIT_ELEMENT(#14394,-3.);
#7961=DERIVED_UNIT_ELEMENT(#8005,1.);
#7962=DERIVED_UNIT_ELEMENT(#14394,-3.);
#7963=DERIVED_UNIT_ELEMENT(#8005,1.);
#7964=DERIVED_UNIT_ELEMENT(#14394,-3.);
#7965=DERIVED_UNIT_ELEMENT(#8005,1.);
#7966=DERIVED_UNIT_ELEMENT(#14394,-3.);
#7967=DERIVED_UNIT_ELEMENT(#8005,1.);
#7968=DERIVED_UNIT_ELEMENT(#14394,-3.);
#7969=DERIVED_UNIT_ELEMENT(#8005,1.);
#7970=DERIVED_UNIT_ELEMENT(#14394,-3.);
#7971=DERIVED_UNIT_ELEMENT(#8005,1.);
#7972=DERIVED_UNIT_ELEMENT(#14394,-3.);
#7973=DERIVED_UNIT_ELEMENT(#8005,1.);
#7974=DERIVED_UNIT_ELEMENT(#14394,-3.);
#7975=DERIVED_UNIT_ELEMENT(#8005,1.);
#7976=DERIVED_UNIT_ELEMENT(#14394,-3.);
#7977=DERIVED_UNIT_ELEMENT(#8005,1.);
#7978=DERIVED_UNIT_ELEMENT(#14394,-3.);
#7979=DERIVED_UNIT_ELEMENT(#8005,1.);
#7980=DERIVED_UNIT_ELEMENT(#14394,-3.);
#7981=DERIVED_UNIT_ELEMENT(#8005,1.);
#7982=DERIVED_UNIT_ELEMENT(#14394,-3.);
#7983=DERIVED_UNIT_ELEMENT(#8005,1.);
#7984=DERIVED_UNIT_ELEMENT(#14394,-3.);
#7985=DERIVED_UNIT_ELEMENT(#8005,1.);
#7986=DERIVED_UNIT_ELEMENT(#14394,-3.);
#7987=DERIVED_UNIT_ELEMENT(#8005,1.);
#7988=DERIVED_UNIT_ELEMENT(#14394,-3.);
#7989=DERIVED_UNIT_ELEMENT(#8005,1.);
#7990=DERIVED_UNIT_ELEMENT(#14394,-3.);
#7991=DERIVED_UNIT_ELEMENT(#8005,1.);
#7992=DERIVED_UNIT_ELEMENT(#14394,-3.);
#7993=DERIVED_UNIT_ELEMENT(#8005,1.);
#7994=DERIVED_UNIT_ELEMENT(#14394,-3.);
#7995=DERIVED_UNIT_ELEMENT(#8005,1.);
#7996=DERIVED_UNIT_ELEMENT(#14394,-3.);
#7997=DERIVED_UNIT_ELEMENT(#8005,1.);
#7998=DERIVED_UNIT_ELEMENT(#14394,-3.);
#7999=DERIVED_UNIT_ELEMENT(#8005,1.);
#8000=DERIVED_UNIT_ELEMENT(#14394,-3.);
#8001=DERIVED_UNIT_ELEMENT(#8005,1.);
#8002=DERIVED_UNIT_ELEMENT(#14394,-3.);
#8003=DERIVED_UNIT_ELEMENT(#8005,1.);
#8004=DERIVED_UNIT_ELEMENT(#14394,-3.);
#8005=(
MASS_UNIT()
NAMED_UNIT(*)
SI_UNIT(.KILO.,.GRAM.)
);
#8006=DERIVED_UNIT((#7921,#7922));
#8007=DERIVED_UNIT((#7923,#7924));
#8008=DERIVED_UNIT((#7925,#7926));
#8009=DERIVED_UNIT((#7927,#7928));
#8010=DERIVED_UNIT((#7929,#7930));
#8011=DERIVED_UNIT((#7931,#7932));
#8012=DERIVED_UNIT((#7933,#7934));
#8013=DERIVED_UNIT((#7935,#7936));
#8014=DERIVED_UNIT((#7937,#7938));
#8015=DERIVED_UNIT((#7939,#7940));
#8016=DERIVED_UNIT((#7941,#7942));
#8017=DERIVED_UNIT((#7943,#7944));
#8018=DERIVED_UNIT((#7945,#7946));
#8019=DERIVED_UNIT((#7947,#7948));
#8020=DERIVED_UNIT((#7949,#7950));
#8021=DERIVED_UNIT((#7951,#7952));
#8022=DERIVED_UNIT((#7953,#7954));
#8023=DERIVED_UNIT((#7955,#7956));
#8024=DERIVED_UNIT((#7957,#7958));
#8025=DERIVED_UNIT((#7959,#7960));
#8026=DERIVED_UNIT((#7961,#7962));
#8027=DERIVED_UNIT((#7963,#7964));
#8028=DERIVED_UNIT((#7965,#7966));
#8029=DERIVED_UNIT((#7967,#7968));
#8030=DERIVED_UNIT((#7969,#7970));
#8031=DERIVED_UNIT((#7971,#7972));
#8032=DERIVED_UNIT((#7973,#7974));
#8033=DERIVED_UNIT((#7975,#7976));
#8034=DERIVED_UNIT((#7977,#7978));
#8035=DERIVED_UNIT((#7979,#7980));
#8036=DERIVED_UNIT((#7981,#7982));
#8037=DERIVED_UNIT((#7983,#7984));
#8038=DERIVED_UNIT((#7985,#7986));
#8039=DERIVED_UNIT((#7987,#7988));
#8040=DERIVED_UNIT((#7989,#7990));
#8041=DERIVED_UNIT((#7991,#7992));
#8042=DERIVED_UNIT((#7993,#7994));
#8043=DERIVED_UNIT((#7995,#7996));
#8044=DERIVED_UNIT((#7997,#7998));
#8045=DERIVED_UNIT((#7999,#8000));
#8046=DERIVED_UNIT((#8001,#8002));
#8047=DERIVED_UNIT((#8003,#8004));
#8048=MEASURE_REPRESENTATION_ITEM('density measure',
POSITIVE_RATIO_MEASURE(7850.),#8006);
#8049=MEASURE_REPRESENTATION_ITEM('density measure',
POSITIVE_RATIO_MEASURE(7850.),#8007);
#8050=MEASURE_REPRESENTATION_ITEM('density measure',
POSITIVE_RATIO_MEASURE(7850.),#8008);
#8051=MEASURE_REPRESENTATION_ITEM('density measure',
POSITIVE_RATIO_MEASURE(7850.),#8009);
#8052=MEASURE_REPRESENTATION_ITEM('density measure',
POSITIVE_RATIO_MEASURE(7850.),#8010);
#8053=MEASURE_REPRESENTATION_ITEM('density measure',
POSITIVE_RATIO_MEASURE(7850.),#8011);
#8054=MEASURE_REPRESENTATION_ITEM('density measure',
POSITIVE_RATIO_MEASURE(7850.),#8012);
#8055=MEASURE_REPRESENTATION_ITEM('density measure',
POSITIVE_RATIO_MEASURE(7850.),#8013);
#8056=MEASURE_REPRESENTATION_ITEM('density measure',
POSITIVE_RATIO_MEASURE(7850.),#8014);
#8057=MEASURE_REPRESENTATION_ITEM('density measure',
POSITIVE_RATIO_MEASURE(7850.),#8015);
#8058=MEASURE_REPRESENTATION_ITEM('density measure',
POSITIVE_RATIO_MEASURE(7850.),#8016);
#8059=MEASURE_REPRESENTATION_ITEM('density measure',
POSITIVE_RATIO_MEASURE(7850.),#8017);
#8060=MEASURE_REPRESENTATION_ITEM('density measure',
POSITIVE_RATIO_MEASURE(7850.),#8018);
#8061=MEASURE_REPRESENTATION_ITEM('density measure',
POSITIVE_RATIO_MEASURE(7850.),#8019);
#8062=MEASURE_REPRESENTATION_ITEM('density measure',
POSITIVE_RATIO_MEASURE(7850.),#8020);
#8063=MEASURE_REPRESENTATION_ITEM('density measure',
POSITIVE_RATIO_MEASURE(7850.),#8021);
#8064=MEASURE_REPRESENTATION_ITEM('density measure',
POSITIVE_RATIO_MEASURE(7850.),#8022);
#8065=MEASURE_REPRESENTATION_ITEM('density measure',
POSITIVE_RATIO_MEASURE(7850.),#8023);
#8066=MEASURE_REPRESENTATION_ITEM('density measure',
POSITIVE_RATIO_MEASURE(7850.),#8024);
#8067=MEASURE_REPRESENTATION_ITEM('density measure',
POSITIVE_RATIO_MEASURE(7850.),#8025);
#8068=MEASURE_REPRESENTATION_ITEM('density measure',
POSITIVE_RATIO_MEASURE(7850.),#8026);
#8069=MEASURE_REPRESENTATION_ITEM('density measure',
POSITIVE_RATIO_MEASURE(7850.),#8027);
#8070=MEASURE_REPRESENTATION_ITEM('density measure',
POSITIVE_RATIO_MEASURE(7850.),#8028);
#8071=MEASURE_REPRESENTATION_ITEM('density measure',
POSITIVE_RATIO_MEASURE(7850.),#8029);
#8072=MEASURE_REPRESENTATION_ITEM('density measure',
POSITIVE_RATIO_MEASURE(7850.),#8030);
#8073=MEASURE_REPRESENTATION_ITEM('density measure',
POSITIVE_RATIO_MEASURE(7850.),#8031);
#8074=MEASURE_REPRESENTATION_ITEM('density measure',
POSITIVE_RATIO_MEASURE(7850.),#8032);
#8075=MEASURE_REPRESENTATION_ITEM('density measure',
POSITIVE_RATIO_MEASURE(7850.),#8033);
#8076=MEASURE_REPRESENTATION_ITEM('density measure',
POSITIVE_RATIO_MEASURE(7850.),#8034);
#8077=MEASURE_REPRESENTATION_ITEM('density measure',
POSITIVE_RATIO_MEASURE(7850.),#8035);
#8078=MEASURE_REPRESENTATION_ITEM('density measure',
POSITIVE_RATIO_MEASURE(7850.),#8036);
#8079=MEASURE_REPRESENTATION_ITEM('density measure',
POSITIVE_RATIO_MEASURE(7850.),#8037);
#8080=MEASURE_REPRESENTATION_ITEM('density measure',
POSITIVE_RATIO_MEASURE(7850.),#8038);
#8081=MEASURE_REPRESENTATION_ITEM('density measure',
POSITIVE_RATIO_MEASURE(7850.),#8039);
#8082=MEASURE_REPRESENTATION_ITEM('density measure',
POSITIVE_RATIO_MEASURE(7850.),#8040);
#8083=MEASURE_REPRESENTATION_ITEM('density measure',
POSITIVE_RATIO_MEASURE(7850.),#8041);
#8084=MEASURE_REPRESENTATION_ITEM('density measure',
POSITIVE_RATIO_MEASURE(7850.),#8042);
#8085=MEASURE_REPRESENTATION_ITEM('density measure',
POSITIVE_RATIO_MEASURE(7850.),#8043);
#8086=MEASURE_REPRESENTATION_ITEM('density measure',
POSITIVE_RATIO_MEASURE(7850.),#8044);
#8087=MEASURE_REPRESENTATION_ITEM('density measure',
POSITIVE_RATIO_MEASURE(7850.),#8045);
#8088=MEASURE_REPRESENTATION_ITEM('density measure',
POSITIVE_RATIO_MEASURE(7850.),#8046);
#8089=MEASURE_REPRESENTATION_ITEM('density measure',
POSITIVE_RATIO_MEASURE(7850.),#8047);
#8090=PROPERTY_DEFINITION_REPRESENTATION(#8300,#8174);
#8091=PROPERTY_DEFINITION_REPRESENTATION(#8301,#8175);
#8092=PROPERTY_DEFINITION_REPRESENTATION(#8302,#8176);
#8093=PROPERTY_DEFINITION_REPRESENTATION(#8303,#8177);
#8094=PROPERTY_DEFINITION_REPRESENTATION(#8304,#8178);
#8095=PROPERTY_DEFINITION_REPRESENTATION(#8305,#8179);
#8096=PROPERTY_DEFINITION_REPRESENTATION(#8306,#8180);
#8097=PROPERTY_DEFINITION_REPRESENTATION(#8307,#8181);
#8098=PROPERTY_DEFINITION_REPRESENTATION(#8308,#8182);
#8099=PROPERTY_DEFINITION_REPRESENTATION(#8309,#8183);
#8100=PROPERTY_DEFINITION_REPRESENTATION(#8310,#8184);
#8101=PROPERTY_DEFINITION_REPRESENTATION(#8311,#8185);
#8102=PROPERTY_DEFINITION_REPRESENTATION(#8312,#8186);
#8103=PROPERTY_DEFINITION_REPRESENTATION(#8313,#8187);
#8104=PROPERTY_DEFINITION_REPRESENTATION(#8314,#8188);
#8105=PROPERTY_DEFINITION_REPRESENTATION(#8315,#8189);
#8106=PROPERTY_DEFINITION_REPRESENTATION(#8316,#8190);
#8107=PROPERTY_DEFINITION_REPRESENTATION(#8317,#8191);
#8108=PROPERTY_DEFINITION_REPRESENTATION(#8318,#8192);
#8109=PROPERTY_DEFINITION_REPRESENTATION(#8319,#8193);
#8110=PROPERTY_DEFINITION_REPRESENTATION(#8320,#8194);
#8111=PROPERTY_DEFINITION_REPRESENTATION(#8321,#8195);
#8112=PROPERTY_DEFINITION_REPRESENTATION(#8322,#8196);
#8113=PROPERTY_DEFINITION_REPRESENTATION(#8323,#8197);
#8114=PROPERTY_DEFINITION_REPRESENTATION(#8324,#8198);
#8115=PROPERTY_DEFINITION_REPRESENTATION(#8325,#8199);
#8116=PROPERTY_DEFINITION_REPRESENTATION(#8326,#8200);
#8117=PROPERTY_DEFINITION_REPRESENTATION(#8327,#8201);
#8118=PROPERTY_DEFINITION_REPRESENTATION(#8328,#8202);
#8119=PROPERTY_DEFINITION_REPRESENTATION(#8329,#8203);
#8120=PROPERTY_DEFINITION_REPRESENTATION(#8330,#8204);
#8121=PROPERTY_DEFINITION_REPRESENTATION(#8331,#8205);
#8122=PROPERTY_DEFINITION_REPRESENTATION(#8332,#8206);
#8123=PROPERTY_DEFINITION_REPRESENTATION(#8333,#8207);
#8124=PROPERTY_DEFINITION_REPRESENTATION(#8334,#8208);
#8125=PROPERTY_DEFINITION_REPRESENTATION(#8335,#8209);
#8126=PROPERTY_DEFINITION_REPRESENTATION(#8336,#8210);
#8127=PROPERTY_DEFINITION_REPRESENTATION(#8337,#8211);
#8128=PROPERTY_DEFINITION_REPRESENTATION(#8338,#8212);
#8129=PROPERTY_DEFINITION_REPRESENTATION(#8339,#8213);
#8130=PROPERTY_DEFINITION_REPRESENTATION(#8340,#8214);
#8131=PROPERTY_DEFINITION_REPRESENTATION(#8341,#8215);
#8132=PROPERTY_DEFINITION_REPRESENTATION(#8342,#8216);
#8133=PROPERTY_DEFINITION_REPRESENTATION(#8343,#8217);
#8134=PROPERTY_DEFINITION_REPRESENTATION(#8344,#8218);
#8135=PROPERTY_DEFINITION_REPRESENTATION(#8345,#8219);
#8136=PROPERTY_DEFINITION_REPRESENTATION(#8346,#8220);
#8137=PROPERTY_DEFINITION_REPRESENTATION(#8347,#8221);
#8138=PROPERTY_DEFINITION_REPRESENTATION(#8348,#8222);
#8139=PROPERTY_DEFINITION_REPRESENTATION(#8349,#8223);
#8140=PROPERTY_DEFINITION_REPRESENTATION(#8350,#8224);
#8141=PROPERTY_DEFINITION_REPRESENTATION(#8351,#8225);
#8142=PROPERTY_DEFINITION_REPRESENTATION(#8352,#8226);
#8143=PROPERTY_DEFINITION_REPRESENTATION(#8353,#8227);
#8144=PROPERTY_DEFINITION_REPRESENTATION(#8354,#8228);
#8145=PROPERTY_DEFINITION_REPRESENTATION(#8355,#8229);
#8146=PROPERTY_DEFINITION_REPRESENTATION(#8356,#8230);
#8147=PROPERTY_DEFINITION_REPRESENTATION(#8357,#8231);
#8148=PROPERTY_DEFINITION_REPRESENTATION(#8358,#8232);
#8149=PROPERTY_DEFINITION_REPRESENTATION(#8359,#8233);
#8150=PROPERTY_DEFINITION_REPRESENTATION(#8360,#8234);
#8151=PROPERTY_DEFINITION_REPRESENTATION(#8361,#8235);
#8152=PROPERTY_DEFINITION_REPRESENTATION(#8362,#8236);
#8153=PROPERTY_DEFINITION_REPRESENTATION(#8363,#8237);
#8154=PROPERTY_DEFINITION_REPRESENTATION(#8364,#8238);
#8155=PROPERTY_DEFINITION_REPRESENTATION(#8365,#8239);
#8156=PROPERTY_DEFINITION_REPRESENTATION(#8366,#8240);
#8157=PROPERTY_DEFINITION_REPRESENTATION(#8367,#8241);
#8158=PROPERTY_DEFINITION_REPRESENTATION(#8368,#8242);
#8159=PROPERTY_DEFINITION_REPRESENTATION(#8369,#8243);
#8160=PROPERTY_DEFINITION_REPRESENTATION(#8370,#8244);
#8161=PROPERTY_DEFINITION_REPRESENTATION(#8371,#8245);
#8162=PROPERTY_DEFINITION_REPRESENTATION(#8372,#8246);
#8163=PROPERTY_DEFINITION_REPRESENTATION(#8373,#8247);
#8164=PROPERTY_DEFINITION_REPRESENTATION(#8374,#8248);
#8165=PROPERTY_DEFINITION_REPRESENTATION(#8375,#8249);
#8166=PROPERTY_DEFINITION_REPRESENTATION(#8376,#8250);
#8167=PROPERTY_DEFINITION_REPRESENTATION(#8377,#8251);
#8168=PROPERTY_DEFINITION_REPRESENTATION(#8378,#8252);
#8169=PROPERTY_DEFINITION_REPRESENTATION(#8379,#8253);
#8170=PROPERTY_DEFINITION_REPRESENTATION(#8380,#8254);
#8171=PROPERTY_DEFINITION_REPRESENTATION(#8381,#8255);
#8172=PROPERTY_DEFINITION_REPRESENTATION(#8382,#8256);
#8173=PROPERTY_DEFINITION_REPRESENTATION(#8383,#8257);
#8174=REPRESENTATION('material name',(#8258),#14347);
#8175=REPRESENTATION('density',(#8048),#14347);
#8176=REPRESENTATION('material name',(#8259),#14348);
#8177=REPRESENTATION('density',(#8049),#14348);
#8178=REPRESENTATION('material name',(#8260),#14349);
#8179=REPRESENTATION('density',(#8050),#14349);
#8180=REPRESENTATION('material name',(#8261),#14350);
#8181=REPRESENTATION('density',(#8051),#14350);
#8182=REPRESENTATION('material name',(#8262),#14351);
#8183=REPRESENTATION('density',(#8052),#14351);
#8184=REPRESENTATION('material name',(#8263),#14352);
#8185=REPRESENTATION('density',(#8053),#14352);
#8186=REPRESENTATION('material name',(#8264),#14353);
#8187=REPRESENTATION('density',(#8054),#14353);
#8188=REPRESENTATION('material name',(#8265),#14354);
#8189=REPRESENTATION('density',(#8055),#14354);
#8190=REPRESENTATION('material name',(#8266),#14355);
#8191=REPRESENTATION('density',(#8056),#14355);
#8192=REPRESENTATION('material name',(#8267),#14356);
#8193=REPRESENTATION('density',(#8057),#14356);
#8194=REPRESENTATION('material name',(#8268),#14357);
#8195=REPRESENTATION('density',(#8058),#14357);
#8196=REPRESENTATION('material name',(#8269),#14359);
#8197=REPRESENTATION('density',(#8059),#14359);
#8198=REPRESENTATION('material name',(#8270),#14360);
#8199=REPRESENTATION('density',(#8060),#14360);
#8200=REPRESENTATION('material name',(#8271),#14361);
#8201=REPRESENTATION('density',(#8061),#14361);
#8202=REPRESENTATION('material name',(#8272),#14362);
#8203=REPRESENTATION('density',(#8062),#14362);
#8204=REPRESENTATION('material name',(#8273),#14363);
#8205=REPRESENTATION('density',(#8063),#14363);
#8206=REPRESENTATION('material name',(#8274),#14364);
#8207=REPRESENTATION('density',(#8064),#14364);
#8208=REPRESENTATION('material name',(#8275),#14365);
#8209=REPRESENTATION('density',(#8065),#14365);
#8210=REPRESENTATION('material name',(#8276),#14366);
#8211=REPRESENTATION('density',(#8066),#14366);
#8212=REPRESENTATION('material name',(#8277),#14367);
#8213=REPRESENTATION('density',(#8067),#14367);
#8214=REPRESENTATION('material name',(#8278),#14368);
#8215=REPRESENTATION('density',(#8068),#14368);
#8216=REPRESENTATION('material name',(#8279),#14369);
#8217=REPRESENTATION('density',(#8069),#14369);
#8218=REPRESENTATION('material name',(#8280),#14370);
#8219=REPRESENTATION('density',(#8070),#14370);
#8220=REPRESENTATION('material name',(#8281),#14371);
#8221=REPRESENTATION('density',(#8071),#14371);
#8222=REPRESENTATION('material name',(#8282),#14373);
#8223=REPRESENTATION('density',(#8072),#14373);
#8224=REPRESENTATION('material name',(#8283),#14374);
#8225=REPRESENTATION('density',(#8073),#14374);
#8226=REPRESENTATION('material name',(#8284),#14375);
#8227=REPRESENTATION('density',(#8074),#14375);
#8228=REPRESENTATION('material name',(#8285),#14376);
#8229=REPRESENTATION('density',(#8075),#14376);
#8230=REPRESENTATION('material name',(#8286),#14378);
#8231=REPRESENTATION('density',(#8076),#14378);
#8232=REPRESENTATION('material name',(#8287),#14379);
#8233=REPRESENTATION('density',(#8077),#14379);
#8234=REPRESENTATION('material name',(#8288),#14380);
#8235=REPRESENTATION('density',(#8078),#14380);
#8236=REPRESENTATION('material name',(#8289),#14381);
#8237=REPRESENTATION('density',(#8079),#14381);
#8238=REPRESENTATION('material name',(#8290),#14382);
#8239=REPRESENTATION('density',(#8080),#14382);
#8240=REPRESENTATION('material name',(#8291),#14383);
#8241=REPRESENTATION('density',(#8081),#14383);
#8242=REPRESENTATION('material name',(#8292),#14384);
#8243=REPRESENTATION('density',(#8082),#14384);
#8244=REPRESENTATION('material name',(#8293),#14385);
#8245=REPRESENTATION('density',(#8083),#14385);
#8246=REPRESENTATION('material name',(#8294),#14386);
#8247=REPRESENTATION('density',(#8084),#14386);
#8248=REPRESENTATION('material name',(#8295),#14387);
#8249=REPRESENTATION('density',(#8085),#14387);
#8250=REPRESENTATION('material name',(#8296),#14388);
#8251=REPRESENTATION('density',(#8086),#14388);
#8252=REPRESENTATION('material name',(#8297),#14389);
#8253=REPRESENTATION('density',(#8087),#14389);
#8254=REPRESENTATION('material name',(#8298),#14390);
#8255=REPRESENTATION('density',(#8088),#14390);
#8256=REPRESENTATION('material name',(#8299),#14391);
#8257=REPRESENTATION('density',(#8089),#14391);
#8258=DESCRIPTIVE_REPRESENTATION_ITEM('Steel','Steel');
#8259=DESCRIPTIVE_REPRESENTATION_ITEM('Steel','Steel');
#8260=DESCRIPTIVE_REPRESENTATION_ITEM('Steel','Steel');
#8261=DESCRIPTIVE_REPRESENTATION_ITEM('Steel','Steel');
#8262=DESCRIPTIVE_REPRESENTATION_ITEM('Steel','Steel');
#8263=DESCRIPTIVE_REPRESENTATION_ITEM('Steel','Steel');
#8264=DESCRIPTIVE_REPRESENTATION_ITEM('Steel','Steel');
#8265=DESCRIPTIVE_REPRESENTATION_ITEM('Steel','Steel');
#8266=DESCRIPTIVE_REPRESENTATION_ITEM('Steel','Steel');
#8267=DESCRIPTIVE_REPRESENTATION_ITEM('Steel','Steel');
#8268=DESCRIPTIVE_REPRESENTATION_ITEM('Steel','Steel');
#8269=DESCRIPTIVE_REPRESENTATION_ITEM('Steel','Steel');
#8270=DESCRIPTIVE_REPRESENTATION_ITEM('Steel','Steel');
#8271=DESCRIPTIVE_REPRESENTATION_ITEM('Steel','Steel');
#8272=DESCRIPTIVE_REPRESENTATION_ITEM('Steel','Steel');
#8273=DESCRIPTIVE_REPRESENTATION_ITEM('Steel','Steel');
#8274=DESCRIPTIVE_REPRESENTATION_ITEM('Steel','Steel');
#8275=DESCRIPTIVE_REPRESENTATION_ITEM('Steel','Steel');
#8276=DESCRIPTIVE_REPRESENTATION_ITEM('Steel','Steel');
#8277=DESCRIPTIVE_REPRESENTATION_ITEM('Steel','Steel');
#8278=DESCRIPTIVE_REPRESENTATION_ITEM('Steel','Steel');
#8279=DESCRIPTIVE_REPRESENTATION_ITEM('Steel','Steel');
#8280=DESCRIPTIVE_REPRESENTATION_ITEM('Steel','Steel');
#8281=DESCRIPTIVE_REPRESENTATION_ITEM('Steel','Steel');
#8282=DESCRIPTIVE_REPRESENTATION_ITEM('Steel','Steel');
#8283=DESCRIPTIVE_REPRESENTATION_ITEM('Steel','Steel');
#8284=DESCRIPTIVE_REPRESENTATION_ITEM('Steel','Steel');
#8285=DESCRIPTIVE_REPRESENTATION_ITEM('Steel','Steel');
#8286=DESCRIPTIVE_REPRESENTATION_ITEM('Steel','Steel');
#8287=DESCRIPTIVE_REPRESENTATION_ITEM('Steel','Steel');
#8288=DESCRIPTIVE_REPRESENTATION_ITEM('Steel','Steel');
#8289=DESCRIPTIVE_REPRESENTATION_ITEM('Steel','Steel');
#8290=DESCRIPTIVE_REPRESENTATION_ITEM('Steel','Steel');
#8291=DESCRIPTIVE_REPRESENTATION_ITEM('Steel','Steel');
#8292=DESCRIPTIVE_REPRESENTATION_ITEM('Steel','Steel');
#8293=DESCRIPTIVE_REPRESENTATION_ITEM('Steel','Steel');
#8294=DESCRIPTIVE_REPRESENTATION_ITEM('Steel','Steel');
#8295=DESCRIPTIVE_REPRESENTATION_ITEM('Steel','Steel');
#8296=DESCRIPTIVE_REPRESENTATION_ITEM('Steel','Steel');
#8297=DESCRIPTIVE_REPRESENTATION_ITEM('Steel','Steel');
#8298=DESCRIPTIVE_REPRESENTATION_ITEM('Steel','Steel');
#8299=DESCRIPTIVE_REPRESENTATION_ITEM('Steel','Steel');
#8300=PROPERTY_DEFINITION('material property','material name',#14633);
#8301=PROPERTY_DEFINITION('material property','density of part',#14633);
#8302=PROPERTY_DEFINITION('material property','material name',#14634);
#8303=PROPERTY_DEFINITION('material property','density of part',#14634);
#8304=PROPERTY_DEFINITION('material property','material name',#14635);
#8305=PROPERTY_DEFINITION('material property','density of part',#14635);
#8306=PROPERTY_DEFINITION('material property','material name',#14636);
#8307=PROPERTY_DEFINITION('material property','density of part',#14636);
#8308=PROPERTY_DEFINITION('material property','material name',#14637);
#8309=PROPERTY_DEFINITION('material property','density of part',#14637);
#8310=PROPERTY_DEFINITION('material property','material name',#14638);
#8311=PROPERTY_DEFINITION('material property','density of part',#14638);
#8312=PROPERTY_DEFINITION('material property','material name',#14639);
#8313=PROPERTY_DEFINITION('material property','density of part',#14639);
#8314=PROPERTY_DEFINITION('material property','material name',#14640);
#8315=PROPERTY_DEFINITION('material property','density of part',#14640);
#8316=PROPERTY_DEFINITION('material property','material name',#14641);
#8317=PROPERTY_DEFINITION('material property','density of part',#14641);
#8318=PROPERTY_DEFINITION('material property','material name',#14642);
#8319=PROPERTY_DEFINITION('material property','density of part',#14642);
#8320=PROPERTY_DEFINITION('material property','material name',#14643);
#8321=PROPERTY_DEFINITION('material property','density of part',#14643);
#8322=PROPERTY_DEFINITION('material property','material name',#14645);
#8323=PROPERTY_DEFINITION('material property','density of part',#14645);
#8324=PROPERTY_DEFINITION('material property','material name',#14646);
#8325=PROPERTY_DEFINITION('material property','density of part',#14646);
#8326=PROPERTY_DEFINITION('material property','material name',#14647);
#8327=PROPERTY_DEFINITION('material property','density of part',#14647);
#8328=PROPERTY_DEFINITION('material property','material name',#14648);
#8329=PROPERTY_DEFINITION('material property','density of part',#14648);
#8330=PROPERTY_DEFINITION('material property','material name',#14649);
#8331=PROPERTY_DEFINITION('material property','density of part',#14649);
#8332=PROPERTY_DEFINITION('material property','material name',#14650);
#8333=PROPERTY_DEFINITION('material property','density of part',#14650);
#8334=PROPERTY_DEFINITION('material property','material name',#14651);
#8335=PROPERTY_DEFINITION('material property','density of part',#14651);
#8336=PROPERTY_DEFINITION('material property','material name',#14652);
#8337=PROPERTY_DEFINITION('material property','density of part',#14652);
#8338=PROPERTY_DEFINITION('material property','material name',#14653);
#8339=PROPERTY_DEFINITION('material property','density of part',#14653);
#8340=PROPERTY_DEFINITION('material property','material name',#14654);
#8341=PROPERTY_DEFINITION('material property','density of part',#14654);
#8342=PROPERTY_DEFINITION('material property','material name',#14655);
#8343=PROPERTY_DEFINITION('material property','density of part',#14655);
#8344=PROPERTY_DEFINITION('material property','material name',#14656);
#8345=PROPERTY_DEFINITION('material property','density of part',#14656);
#8346=PROPERTY_DEFINITION('material property','material name',#14657);
#8347=PROPERTY_DEFINITION('material property','density of part',#14657);
#8348=PROPERTY_DEFINITION('material property','material name',#14659);
#8349=PROPERTY_DEFINITION('material property','density of part',#14659);
#8350=PROPERTY_DEFINITION('material property','material name',#14660);
#8351=PROPERTY_DEFINITION('material property','density of part',#14660);
#8352=PROPERTY_DEFINITION('material property','material name',#14661);
#8353=PROPERTY_DEFINITION('material property','density of part',#14661);
#8354=PROPERTY_DEFINITION('material property','material name',#14662);
#8355=PROPERTY_DEFINITION('material property','density of part',#14662);
#8356=PROPERTY_DEFINITION('material property','material name',#14664);
#8357=PROPERTY_DEFINITION('material property','density of part',#14664);
#8358=PROPERTY_DEFINITION('material property','material name',#14665);
#8359=PROPERTY_DEFINITION('material property','density of part',#14665);
#8360=PROPERTY_DEFINITION('material property','material name',#14666);
#8361=PROPERTY_DEFINITION('material property','density of part',#14666);
#8362=PROPERTY_DEFINITION('material property','material name',#14667);
#8363=PROPERTY_DEFINITION('material property','density of part',#14667);
#8364=PROPERTY_DEFINITION('material property','material name',#14668);
#8365=PROPERTY_DEFINITION('material property','density of part',#14668);
#8366=PROPERTY_DEFINITION('material property','material name',#14669);
#8367=PROPERTY_DEFINITION('material property','density of part',#14669);
#8368=PROPERTY_DEFINITION('material property','material name',#14670);
#8369=PROPERTY_DEFINITION('material property','density of part',#14670);
#8370=PROPERTY_DEFINITION('material property','material name',#14671);
#8371=PROPERTY_DEFINITION('material property','density of part',#14671);
#8372=PROPERTY_DEFINITION('material property','material name',#14672);
#8373=PROPERTY_DEFINITION('material property','density of part',#14672);
#8374=PROPERTY_DEFINITION('material property','material name',#14673);
#8375=PROPERTY_DEFINITION('material property','density of part',#14673);
#8376=PROPERTY_DEFINITION('material property','material name',#14674);
#8377=PROPERTY_DEFINITION('material property','density of part',#14674);
#8378=PROPERTY_DEFINITION('material property','material name',#14675);
#8379=PROPERTY_DEFINITION('material property','density of part',#14675);
#8380=PROPERTY_DEFINITION('material property','material name',#14676);
#8381=PROPERTY_DEFINITION('material property','density of part',#14676);
#8382=PROPERTY_DEFINITION('material property','material name',#14677);
#8383=PROPERTY_DEFINITION('material property','density of part',#14677);
#8384=AXIS2_PLACEMENT_3D('',#11920,#9381,#9382);
#8385=AXIS2_PLACEMENT_3D('',#11921,#9383,#9384);
#8386=AXIS2_PLACEMENT_3D('',#11922,#9385,#9386);
#8387=AXIS2_PLACEMENT_3D('',#11923,#9387,#9388);
#8388=AXIS2_PLACEMENT_3D('',#11925,#9389,#9390);
#8389=AXIS2_PLACEMENT_3D('',#11928,#9392,#9393);
#8390=AXIS2_PLACEMENT_3D('',#11929,#9394,#9395);
#8391=AXIS2_PLACEMENT_3D('',#11930,#9396,#9397);
#8392=AXIS2_PLACEMENT_3D('',#11932,#9398,#9399);
#8393=AXIS2_PLACEMENT_3D('',#11935,#9401,#9402);
#8394=AXIS2_PLACEMENT_3D('',#11936,#9403,#9404);
#8395=AXIS2_PLACEMENT_3D('',#11937,#9405,#9406);
#8396=AXIS2_PLACEMENT_3D('',#11941,#9408,#9409);
#8397=AXIS2_PLACEMENT_3D('',#11942,#9410,#9411);
#8398=AXIS2_PLACEMENT_3D('',#11945,#9413,#9414);
#8399=AXIS2_PLACEMENT_3D('',#11946,#9415,#9416);
#8400=AXIS2_PLACEMENT_3D('',#11948,#9417,#9418);
#8401=AXIS2_PLACEMENT_3D('',#11949,#9419,#9420);
#8402=AXIS2_PLACEMENT_3D('',#11950,#9421,#9422);
#8403=AXIS2_PLACEMENT_3D('',#11955,#9425,#9426);
#8404=AXIS2_PLACEMENT_3D('',#11957,#9427,#9428);
#8405=AXIS2_PLACEMENT_3D('',#11961,#9430,#9431);
#8406=AXIS2_PLACEMENT_3D('',#11965,#9433,#9434);
#8407=AXIS2_PLACEMENT_3D('',#11968,#9436,#9437);
#8408=AXIS2_PLACEMENT_3D('',#11969,#9438,#9439);
#8409=AXIS2_PLACEMENT_3D('',#11970,#9440,#9441);
#8410=AXIS2_PLACEMENT_3D('',#11972,#9442,#9443);
#8411=AXIS2_PLACEMENT_3D('',#11973,#9444,#9445);
#8412=AXIS2_PLACEMENT_3D('',#11974,#9446,#9447);
#8413=AXIS2_PLACEMENT_3D('',#11975,#9448,#9449);
#8414=AXIS2_PLACEMENT_3D('',#11976,#9450,#9451);
#8415=AXIS2_PLACEMENT_3D('',#11977,#9452,#9453);
#8416=AXIS2_PLACEMENT_3D('',#11979,#9455,#9456);
#8417=AXIS2_PLACEMENT_3D('',#11980,#9457,#9458);
#8418=AXIS2_PLACEMENT_3D('',#11981,#9459,#9460);
#8419=AXIS2_PLACEMENT_3D('',#11982,#9461,#9462);
#8420=AXIS2_PLACEMENT_3D('',#11983,#9463,#9464);
#8421=AXIS2_PLACEMENT_3D('',#11984,#9465,#9466);
#8422=AXIS2_PLACEMENT_3D('',#11987,#9468,#9469);
#8423=AXIS2_PLACEMENT_3D('',#11988,#9470,#9471);
#8424=AXIS2_PLACEMENT_3D('',#11989,#9472,#9473);
#8425=AXIS2_PLACEMENT_3D('',#11990,#9474,#9475);
#8426=AXIS2_PLACEMENT_3D('',#11992,#9476,#9477);
#8427=AXIS2_PLACEMENT_3D('',#11995,#9479,#9480);
#8428=AXIS2_PLACEMENT_3D('',#11996,#9481,#9482);
#8429=AXIS2_PLACEMENT_3D('',#11997,#9483,#9484);
#8430=AXIS2_PLACEMENT_3D('',#11998,#9485,#9486);
#8431=AXIS2_PLACEMENT_3D('',#12000,#9487,#9488);
#8432=AXIS2_PLACEMENT_3D('',#12003,#9490,#9491);
#8433=AXIS2_PLACEMENT_3D('',#12004,#9492,#9493);
#8434=AXIS2_PLACEMENT_3D('',#12005,#9494,#9495);
#8435=AXIS2_PLACEMENT_3D('',#12007,#9496,#9497);
#8436=AXIS2_PLACEMENT_3D('',#12010,#9499,#9500);
#8437=AXIS2_PLACEMENT_3D('',#12011,#9501,#9502);
#8438=AXIS2_PLACEMENT_3D('',#12013,#9503,#9504);
#8439=AXIS2_PLACEMENT_3D('',#12016,#9506,#9507);
#8440=AXIS2_PLACEMENT_3D('',#12017,#9508,#9509);
#8441=AXIS2_PLACEMENT_3D('',#12019,#9510,#9511);
#8442=AXIS2_PLACEMENT_3D('',#12022,#9513,#9514);
#8443=AXIS2_PLACEMENT_3D('',#12023,#9515,#9516);
#8444=AXIS2_PLACEMENT_3D('',#12025,#9517,#9518);
#8445=AXIS2_PLACEMENT_3D('',#12028,#9520,#9521);
#8446=AXIS2_PLACEMENT_3D('',#12029,#9522,#9523);
#8447=AXIS2_PLACEMENT_3D('',#12031,#9524,#9525);
#8448=AXIS2_PLACEMENT_3D('',#12034,#9527,#9528);
#8449=AXIS2_PLACEMENT_3D('',#12035,#9529,#9530);
#8450=AXIS2_PLACEMENT_3D('',#12036,#9531,#9532);
#8451=AXIS2_PLACEMENT_3D('',#12045,#9537,#9538);
#8452=AXIS2_PLACEMENT_3D('',#12051,#9542,#9543);
#8453=AXIS2_PLACEMENT_3D('',#12057,#9547,#9548);
#8454=AXIS2_PLACEMENT_3D('',#12060,#9551,#9552);
#8455=AXIS2_PLACEMENT_3D('',#12061,#9553,#9554);
#8456=AXIS2_PLACEMENT_3D('',#12062,#9555,#9556);
#8457=AXIS2_PLACEMENT_3D('',#12063,#9557,#9558);
#8458=AXIS2_PLACEMENT_3D('',#12065,#9559,#9560);
#8459=AXIS2_PLACEMENT_3D('',#12068,#9562,#9563);
#8460=AXIS2_PLACEMENT_3D('',#12069,#9564,#9565);
#8461=AXIS2_PLACEMENT_3D('',#12078,#9570,#9571);
#8462=AXIS2_PLACEMENT_3D('',#12079,#9572,#9573);
#8463=AXIS2_PLACEMENT_3D('',#12081,#9574,#9575);
#8464=AXIS2_PLACEMENT_3D('',#12082,#9576,#9577);
#8465=AXIS2_PLACEMENT_3D('',#12083,#9578,#9579);
#8466=AXIS2_PLACEMENT_3D('',#12084,#9580,#9581);
#8467=AXIS2_PLACEMENT_3D('',#12086,#9582,#9583);
#8468=AXIS2_PLACEMENT_3D('',#12089,#9585,#9586);
#8469=AXIS2_PLACEMENT_3D('',#12090,#9587,#9588);
#8470=AXIS2_PLACEMENT_3D('',#12092,#9589,#9590);
#8471=AXIS2_PLACEMENT_3D('',#12093,#9591,#9592);
#8472=AXIS2_PLACEMENT_3D('',#12095,#9593,#9594);
#8473=AXIS2_PLACEMENT_3D('',#12096,#9595,#9596);
#8474=AXIS2_PLACEMENT_3D('',#12098,#9598,#9599);
#8475=AXIS2_PLACEMENT_3D('',#12101,#9601,#9602);
#8476=AXIS2_PLACEMENT_3D('',#12102,#9603,#9604);
#8477=AXIS2_PLACEMENT_3D('',#12104,#9605,#9606);
#8478=AXIS2_PLACEMENT_3D('',#12105,#9607,#9608);
#8479=AXIS2_PLACEMENT_3D('',#12118,#9615,#9616);
#8480=AXIS2_PLACEMENT_3D('',#12127,#9621,#9622);
#8481=AXIS2_PLACEMENT_3D('',#12134,#9627,#9628);
#8482=AXIS2_PLACEMENT_3D('',#12138,#9631,#9632);
#8483=AXIS2_PLACEMENT_3D('',#12143,#9636,#9637);
#8484=AXIS2_PLACEMENT_3D('',#12144,#9638,#9639);
#8485=AXIS2_PLACEMENT_3D('',#12150,#9643,#9644);
#8486=AXIS2_PLACEMENT_3D('',#12154,#9647,#9648);
#8487=AXIS2_PLACEMENT_3D('',#12168,#9655,#9656);
#8488=AXIS2_PLACEMENT_3D('',#12169,#9657,#9658);
#8489=AXIS2_PLACEMENT_3D('',#12172,#9661,#9662);
#8490=AXIS2_PLACEMENT_3D('',#12176,#9665,#9666);
#8491=AXIS2_PLACEMENT_3D('',#12179,#9669,#9670);
#8492=AXIS2_PLACEMENT_3D('',#12181,#9672,#9673);
#8493=AXIS2_PLACEMENT_3D('',#12183,#9675,#9676);
#8494=AXIS2_PLACEMENT_3D('',#12184,#9677,#9678);
#8495=AXIS2_PLACEMENT_3D('',#12185,#9679,#9680);
#8496=AXIS2_PLACEMENT_3D('',#12188,#9682,#9683);
#8497=AXIS2_PLACEMENT_3D('',#12189,#9684,#9685);
#8498=AXIS2_PLACEMENT_3D('',#12192,#9687,#9688);
#8499=AXIS2_PLACEMENT_3D('',#12193,#9689,#9690);
#8500=AXIS2_PLACEMENT_3D('',#12194,#9691,#9692);
#8501=AXIS2_PLACEMENT_3D('',#12195,#9693,#9694);
#8502=AXIS2_PLACEMENT_3D('',#12197,#9695,#9696);
#8503=AXIS2_PLACEMENT_3D('',#12200,#9698,#9699);
#8504=AXIS2_PLACEMENT_3D('',#12202,#9700,#9701);
#8505=AXIS2_PLACEMENT_3D('',#12204,#9703,#9704);
#8506=AXIS2_PLACEMENT_3D('',#12206,#9705,#9706);
#8507=AXIS2_PLACEMENT_3D('',#12208,#9708,#9709);
#8508=AXIS2_PLACEMENT_3D('',#12210,#9710,#9711);
#8509=AXIS2_PLACEMENT_3D('',#12211,#9712,#9713);
#8510=AXIS2_PLACEMENT_3D('',#12213,#9714,#9715);
#8511=AXIS2_PLACEMENT_3D('',#12215,#9717,#9718);
#8512=AXIS2_PLACEMENT_3D('',#12216,#9719,#9720);
#8513=AXIS2_PLACEMENT_3D('',#12217,#9721,#9722);
#8514=AXIS2_PLACEMENT_3D('',#12219,#9723,#9724);
#8515=AXIS2_PLACEMENT_3D('',#12222,#9726,#9727);
#8516=AXIS2_PLACEMENT_3D('',#12223,#9728,#9729);
#8517=AXIS2_PLACEMENT_3D('',#12224,#9730,#9731);
#8518=AXIS2_PLACEMENT_3D('',#12226,#9732,#9733);
#8519=AXIS2_PLACEMENT_3D('',#12229,#9735,#9736);
#8520=AXIS2_PLACEMENT_3D('',#12230,#9737,#9738);
#8521=AXIS2_PLACEMENT_3D('',#12231,#9739,#9740);
#8522=AXIS2_PLACEMENT_3D('',#12235,#9742,#9743);
#8523=AXIS2_PLACEMENT_3D('',#12236,#9744,#9745);
#8524=AXIS2_PLACEMENT_3D('',#12239,#9747,#9748);
#8525=AXIS2_PLACEMENT_3D('',#12240,#9749,#9750);
#8526=AXIS2_PLACEMENT_3D('',#12243,#9752,#9753);
#8527=AXIS2_PLACEMENT_3D('',#12244,#9754,#9755);
#8528=AXIS2_PLACEMENT_3D('',#12249,#9757,#9758);
#8529=AXIS2_PLACEMENT_3D('',#12253,#9760,#9761);
#8530=AXIS2_PLACEMENT_3D('',#12257,#9763,#9764);
#8531=AXIS2_PLACEMENT_3D('',#12259,#9765,#9766);
#8532=AXIS2_PLACEMENT_3D('',#12263,#9769,#9770);
#8533=AXIS2_PLACEMENT_3D('',#12264,#9771,#9772);
#8534=AXIS2_PLACEMENT_3D('',#12265,#9773,#9774);
#8535=AXIS2_PLACEMENT_3D('',#12266,#9775,#9776);
#8536=AXIS2_PLACEMENT_3D('',#12267,#9777,#9778);
#8537=AXIS2_PLACEMENT_3D('',#12268,#9779,#9780);
#8538=AXIS2_PLACEMENT_3D('',#12269,#9781,#9782);
#8539=AXIS2_PLACEMENT_3D('',#12270,#9783,#9784);
#8540=AXIS2_PLACEMENT_3D('',#12271,#9785,#9786);
#8541=AXIS2_PLACEMENT_3D('',#12272,#9787,#9788);
#8542=AXIS2_PLACEMENT_3D('',#12273,#9789,#9790);
#8543=AXIS2_PLACEMENT_3D('',#12274,#9791,#9792);
#8544=AXIS2_PLACEMENT_3D('',#12275,#9793,#9794);
#8545=AXIS2_PLACEMENT_3D('',#12276,#9795,#9796);
#8546=AXIS2_PLACEMENT_3D('',#12277,#9797,#9798);
#8547=AXIS2_PLACEMENT_3D('',#12278,#9799,#9800);
#8548=AXIS2_PLACEMENT_3D('',#12279,#9801,#9802);
#8549=AXIS2_PLACEMENT_3D('',#12280,#9803,#9804);
#8550=AXIS2_PLACEMENT_3D('',#12281,#9805,#9806);
#8551=AXIS2_PLACEMENT_3D('',#12284,#9808,#9809);
#8552=AXIS2_PLACEMENT_3D('',#12285,#9810,#9811);
#8553=AXIS2_PLACEMENT_3D('',#12287,#9812,#9813);
#8554=AXIS2_PLACEMENT_3D('',#12288,#9814,#9815);
#8555=AXIS2_PLACEMENT_3D('',#12289,#9816,#9817);
#8556=AXIS2_PLACEMENT_3D('',#12291,#9818,#9819);
#8557=AXIS2_PLACEMENT_3D('',#12294,#9821,#9822);
#8558=AXIS2_PLACEMENT_3D('',#12295,#9823,#9824);
#8559=AXIS2_PLACEMENT_3D('',#12296,#9825,#9826);
#8560=AXIS2_PLACEMENT_3D('',#12298,#9827,#9828);
#8561=AXIS2_PLACEMENT_3D('',#12301,#9830,#9831);
#8562=AXIS2_PLACEMENT_3D('',#12302,#9832,#9833);
#8563=AXIS2_PLACEMENT_3D('',#12304,#9834,#9835);
#8564=AXIS2_PLACEMENT_3D('',#12307,#9837,#9838);
#8565=AXIS2_PLACEMENT_3D('',#12308,#9839,#9840);
#8566=AXIS2_PLACEMENT_3D('',#12310,#9841,#9842);
#8567=AXIS2_PLACEMENT_3D('',#12313,#9844,#9845);
#8568=AXIS2_PLACEMENT_3D('',#12314,#9846,#9847);
#8569=AXIS2_PLACEMENT_3D('',#12316,#9848,#9849);
#8570=AXIS2_PLACEMENT_3D('',#12319,#9851,#9852);
#8571=AXIS2_PLACEMENT_3D('',#12320,#9853,#9854);
#8572=AXIS2_PLACEMENT_3D('',#12322,#9855,#9856);
#8573=AXIS2_PLACEMENT_3D('',#12324,#9858,#9859);
#8574=AXIS2_PLACEMENT_3D('',#12333,#9864,#9865);
#8575=AXIS2_PLACEMENT_3D('',#12339,#9869,#9870);
#8576=AXIS2_PLACEMENT_3D('',#12345,#9874,#9875);
#8577=AXIS2_PLACEMENT_3D('',#12348,#9878,#9879);
#8578=AXIS2_PLACEMENT_3D('',#12349,#9880,#9881);
#8579=AXIS2_PLACEMENT_3D('',#12350,#9882,#9883);
#8580=AXIS2_PLACEMENT_3D('',#12351,#9884,#9885);
#8581=AXIS2_PLACEMENT_3D('',#12353,#9886,#9887);
#8582=AXIS2_PLACEMENT_3D('',#12356,#9889,#9890);
#8583=AXIS2_PLACEMENT_3D('',#12357,#9891,#9892);
#8584=AXIS2_PLACEMENT_3D('',#12366,#9897,#9898);
#8585=AXIS2_PLACEMENT_3D('',#12367,#9899,#9900);
#8586=AXIS2_PLACEMENT_3D('',#12369,#9901,#9902);
#8587=AXIS2_PLACEMENT_3D('',#12370,#9903,#9904);
#8588=AXIS2_PLACEMENT_3D('',#12371,#9905,#9906);
#8589=AXIS2_PLACEMENT_3D('',#12372,#9907,#9908);
#8590=AXIS2_PLACEMENT_3D('',#12374,#9909,#9910);
#8591=AXIS2_PLACEMENT_3D('',#12377,#9912,#9913);
#8592=AXIS2_PLACEMENT_3D('',#12378,#9914,#9915);
#8593=AXIS2_PLACEMENT_3D('',#12380,#9916,#9917);
#8594=AXIS2_PLACEMENT_3D('',#12381,#9918,#9919);
#8595=AXIS2_PLACEMENT_3D('',#12383,#9920,#9921);
#8596=AXIS2_PLACEMENT_3D('',#12384,#9922,#9923);
#8597=AXIS2_PLACEMENT_3D('',#12386,#9925,#9926);
#8598=AXIS2_PLACEMENT_3D('',#12389,#9928,#9929);
#8599=AXIS2_PLACEMENT_3D('',#12390,#9930,#9931);
#8600=AXIS2_PLACEMENT_3D('',#12392,#9932,#9933);
#8601=AXIS2_PLACEMENT_3D('',#12393,#9934,#9935);
#8602=AXIS2_PLACEMENT_3D('',#12406,#9942,#9943);
#8603=AXIS2_PLACEMENT_3D('',#12415,#9948,#9949);
#8604=AXIS2_PLACEMENT_3D('',#12422,#9954,#9955);
#8605=AXIS2_PLACEMENT_3D('',#12426,#9958,#9959);
#8606=AXIS2_PLACEMENT_3D('',#12431,#9963,#9964);
#8607=AXIS2_PLACEMENT_3D('',#12432,#9965,#9966);
#8608=AXIS2_PLACEMENT_3D('',#12438,#9970,#9971);
#8609=AXIS2_PLACEMENT_3D('',#12442,#9974,#9975);
#8610=AXIS2_PLACEMENT_3D('',#12456,#9982,#9983);
#8611=AXIS2_PLACEMENT_3D('',#12457,#9984,#9985);
#8612=AXIS2_PLACEMENT_3D('',#12460,#9988,#9989);
#8613=AXIS2_PLACEMENT_3D('',#12464,#9992,#9993);
#8614=AXIS2_PLACEMENT_3D('',#12467,#9996,#9997);
#8615=AXIS2_PLACEMENT_3D('',#12469,#9999,#10000);
#8616=AXIS2_PLACEMENT_3D('',#12471,#10002,#10003);
#8617=AXIS2_PLACEMENT_3D('',#12472,#10004,#10005);
#8618=AXIS2_PLACEMENT_3D('',#12473,#10006,#10007);
#8619=AXIS2_PLACEMENT_3D('',#12476,#10009,#10010);
#8620=AXIS2_PLACEMENT_3D('',#12477,#10011,#10012);
#8621=AXIS2_PLACEMENT_3D('',#12480,#10014,#10015);
#8622=AXIS2_PLACEMENT_3D('',#12481,#10016,#10017);
#8623=AXIS2_PLACEMENT_3D('',#12482,#10018,#10019);
#8624=AXIS2_PLACEMENT_3D('',#12483,#10020,#10021);
#8625=AXIS2_PLACEMENT_3D('',#12485,#10022,#10023);
#8626=AXIS2_PLACEMENT_3D('',#12488,#10025,#10026);
#8627=AXIS2_PLACEMENT_3D('',#12490,#10027,#10028);
#8628=AXIS2_PLACEMENT_3D('',#12492,#10030,#10031);
#8629=AXIS2_PLACEMENT_3D('',#12494,#10032,#10033);
#8630=AXIS2_PLACEMENT_3D('',#12496,#10035,#10036);
#8631=AXIS2_PLACEMENT_3D('',#12498,#10037,#10038);
#8632=AXIS2_PLACEMENT_3D('',#12499,#10039,#10040);
#8633=AXIS2_PLACEMENT_3D('',#12501,#10041,#10042);
#8634=AXIS2_PLACEMENT_3D('',#12503,#10044,#10045);
#8635=AXIS2_PLACEMENT_3D('',#12504,#10046,#10047);
#8636=AXIS2_PLACEMENT_3D('',#12505,#10048,#10049);
#8637=AXIS2_PLACEMENT_3D('',#12507,#10050,#10051);
#8638=AXIS2_PLACEMENT_3D('',#12510,#10053,#10054);
#8639=AXIS2_PLACEMENT_3D('',#12511,#10055,#10056);
#8640=AXIS2_PLACEMENT_3D('',#12513,#10057,#10058);
#8641=AXIS2_PLACEMENT_3D('',#12516,#10060,#10061);
#8642=AXIS2_PLACEMENT_3D('',#12517,#10062,#10063);
#8643=AXIS2_PLACEMENT_3D('',#12518,#10064,#10065);
#8644=AXIS2_PLACEMENT_3D('',#12519,#10066,#10067);
#8645=AXIS2_PLACEMENT_3D('',#12520,#10068,#10069);
#8646=AXIS2_PLACEMENT_3D('',#12522,#10070,#10071);
#8647=AXIS2_PLACEMENT_3D('',#12525,#10073,#10074);
#8648=AXIS2_PLACEMENT_3D('',#12526,#10075,#10076);
#8649=AXIS2_PLACEMENT_3D('',#12528,#10077,#10078);
#8650=AXIS2_PLACEMENT_3D('',#12531,#10080,#10081);
#8651=AXIS2_PLACEMENT_3D('',#12532,#10082,#10083);
#8652=AXIS2_PLACEMENT_3D('',#12533,#10084,#10085);
#8653=AXIS2_PLACEMENT_3D('',#12534,#10086,#10087);
#8654=AXIS2_PLACEMENT_3D('',#12535,#10088,#10089);
#8655=AXIS2_PLACEMENT_3D('',#12537,#10090,#10091);
#8656=AXIS2_PLACEMENT_3D('',#12540,#10093,#10094);
#8657=AXIS2_PLACEMENT_3D('',#12541,#10095,#10096);
#8658=AXIS2_PLACEMENT_3D('',#12543,#10097,#10098);
#8659=AXIS2_PLACEMENT_3D('',#12546,#10100,#10101);
#8660=AXIS2_PLACEMENT_3D('',#12547,#10102,#10103);
#8661=AXIS2_PLACEMENT_3D('',#12548,#10104,#10105);
#8662=AXIS2_PLACEMENT_3D('',#12549,#10106,#10107);
#8663=AXIS2_PLACEMENT_3D('',#12550,#10108,#10109);
#8664=AXIS2_PLACEMENT_3D('',#12552,#10110,#10111);
#8665=AXIS2_PLACEMENT_3D('',#12555,#10113,#10114);
#8666=AXIS2_PLACEMENT_3D('',#12556,#10115,#10116);
#8667=AXIS2_PLACEMENT_3D('',#12558,#10117,#10118);
#8668=AXIS2_PLACEMENT_3D('',#12559,#10119,#10120);
#8669=AXIS2_PLACEMENT_3D('',#12561,#10121,#10122);
#8670=AXIS2_PLACEMENT_3D('',#12564,#10124,#10125);
#8671=AXIS2_PLACEMENT_3D('',#12565,#10126,#10127);
#8672=AXIS2_PLACEMENT_3D('',#12567,#10128,#10129);
#8673=AXIS2_PLACEMENT_3D('',#12568,#10130,#10131);
#8674=AXIS2_PLACEMENT_3D('',#12570,#10132,#10133);
#8675=AXIS2_PLACEMENT_3D('',#12572,#10135,#10136);
#8676=AXIS2_PLACEMENT_3D('',#12574,#10137,#10138);
#8677=AXIS2_PLACEMENT_3D('',#12576,#10140,#10141);
#8678=AXIS2_PLACEMENT_3D('',#12578,#10142,#10143);
#8679=AXIS2_PLACEMENT_3D('',#12581,#10145,#10146);
#8680=AXIS2_PLACEMENT_3D('',#12582,#10147,#10148);
#8681=AXIS2_PLACEMENT_3D('',#12584,#10149,#10150);
#8682=AXIS2_PLACEMENT_3D('',#12585,#10151,#10152);
#8683=AXIS2_PLACEMENT_3D('',#12587,#10153,#10154);
#8684=AXIS2_PLACEMENT_3D('',#12590,#10156,#10157);
#8685=AXIS2_PLACEMENT_3D('',#12591,#10158,#10159);
#8686=AXIS2_PLACEMENT_3D('',#12593,#10160,#10161);
#8687=AXIS2_PLACEMENT_3D('',#12594,#10162,#10163);
#8688=AXIS2_PLACEMENT_3D('',#12597,#10165,#10166);
#8689=AXIS2_PLACEMENT_3D('',#12598,#10167,#10168);
#8690=AXIS2_PLACEMENT_3D('',#12601,#10170,#10171);
#8691=AXIS2_PLACEMENT_3D('',#12602,#10172,#10173);
#8692=AXIS2_PLACEMENT_3D('',#12611,#10178,#10179);
#8693=AXIS2_PLACEMENT_3D('',#12617,#10183,#10184);
#8694=AXIS2_PLACEMENT_3D('',#12623,#10188,#10189);
#8695=AXIS2_PLACEMENT_3D('',#12626,#10192,#10193);
#8696=AXIS2_PLACEMENT_3D('',#12627,#10194,#10195);
#8697=AXIS2_PLACEMENT_3D('',#12628,#10196,#10197);
#8698=AXIS2_PLACEMENT_3D('',#12629,#10198,#10199);
#8699=AXIS2_PLACEMENT_3D('',#12631,#10200,#10201);
#8700=AXIS2_PLACEMENT_3D('',#12632,#10202,#10203);
#8701=AXIS2_PLACEMENT_3D('',#12634,#10204,#10205);
#8702=AXIS2_PLACEMENT_3D('',#12636,#10207,#10208);
#8703=AXIS2_PLACEMENT_3D('',#12638,#10209,#10210);
#8704=AXIS2_PLACEMENT_3D('',#12640,#10212,#10213);
#8705=AXIS2_PLACEMENT_3D('',#12642,#10214,#10215);
#8706=AXIS2_PLACEMENT_3D('',#12644,#10217,#10218);
#8707=AXIS2_PLACEMENT_3D('',#12646,#10219,#10220);
#8708=AXIS2_PLACEMENT_3D('',#12647,#10221,#10222);
#8709=AXIS2_PLACEMENT_3D('',#12649,#10223,#10224);
#8710=AXIS2_PLACEMENT_3D('',#12651,#10226,#10227);
#8711=AXIS2_PLACEMENT_3D('',#12653,#10228,#10229);
#8712=AXIS2_PLACEMENT_3D('',#12655,#10231,#10232);
#8713=AXIS2_PLACEMENT_3D('',#12657,#10233,#10234);
#8714=AXIS2_PLACEMENT_3D('',#12659,#10236,#10237);
#8715=AXIS2_PLACEMENT_3D('',#12660,#10238,#10239);
#8716=AXIS2_PLACEMENT_3D('',#12669,#10244,#10245);
#8717=AXIS2_PLACEMENT_3D('',#12675,#10249,#10250);
#8718=AXIS2_PLACEMENT_3D('',#12681,#10254,#10255);
#8719=AXIS2_PLACEMENT_3D('',#12687,#10259,#10260);
#8720=AXIS2_PLACEMENT_3D('',#12693,#10264,#10265);
#8721=AXIS2_PLACEMENT_3D('',#12696,#10268,#10269);
#8722=AXIS2_PLACEMENT_3D('',#12697,#10270,#10271);
#8723=AXIS2_PLACEMENT_3D('',#12698,#10272,#10273);
#8724=AXIS2_PLACEMENT_3D('',#12699,#10274,#10275);
#8725=AXIS2_PLACEMENT_3D('',#12700,#10276,#10277);
#8726=AXIS2_PLACEMENT_3D('',#12702,#10278,#10279);
#8727=AXIS2_PLACEMENT_3D('',#12705,#10281,#10282);
#8728=AXIS2_PLACEMENT_3D('',#12706,#10283,#10284);
#8729=AXIS2_PLACEMENT_3D('',#12708,#10285,#10286);
#8730=AXIS2_PLACEMENT_3D('',#12709,#10287,#10288);
#8731=AXIS2_PLACEMENT_3D('',#12723,#10295,#10296);
#8732=AXIS2_PLACEMENT_3D('',#12724,#10297,#10298);
#8733=AXIS2_PLACEMENT_3D('',#12738,#10305,#10306);
#8734=AXIS2_PLACEMENT_3D('',#12739,#10307,#10308);
#8735=AXIS2_PLACEMENT_3D('',#12742,#10311,#10312);
#8736=AXIS2_PLACEMENT_3D('',#12744,#10314,#10315);
#8737=AXIS2_PLACEMENT_3D('',#12746,#10317,#10318);
#8738=AXIS2_PLACEMENT_3D('',#12748,#10320,#10321);
#8739=AXIS2_PLACEMENT_3D('',#12750,#10323,#10324);
#8740=AXIS2_PLACEMENT_3D('',#12751,#10325,#10326);
#8741=AXIS2_PLACEMENT_3D('',#12753,#10327,#10328);
#8742=AXIS2_PLACEMENT_3D('',#12754,#10329,#10330);
#8743=AXIS2_PLACEMENT_3D('',#12757,#10332,#10333);
#8744=AXIS2_PLACEMENT_3D('',#12758,#10334,#10335);
#8745=AXIS2_PLACEMENT_3D('',#12760,#10336,#10337);
#8746=AXIS2_PLACEMENT_3D('',#12761,#10338,#10339);
#8747=AXIS2_PLACEMENT_3D('',#12763,#10341,#10342);
#8748=AXIS2_PLACEMENT_3D('',#12765,#10343,#10344);
#8749=AXIS2_PLACEMENT_3D('',#12767,#10346,#10347);
#8750=AXIS2_PLACEMENT_3D('',#12769,#10348,#10349);
#8751=AXIS2_PLACEMENT_3D('',#12770,#10350,#10351);
#8752=AXIS2_PLACEMENT_3D('',#12772,#10353,#10354);
#8753=AXIS2_PLACEMENT_3D('',#12773,#10355,#10356);
#8754=AXIS2_PLACEMENT_3D('',#12775,#10357,#10358);
#8755=AXIS2_PLACEMENT_3D('',#12777,#10359,#10360);
#8756=AXIS2_PLACEMENT_3D('',#12778,#10361,#10362);
#8757=AXIS2_PLACEMENT_3D('',#12780,#10363,#10364);
#8758=AXIS2_PLACEMENT_3D('',#12782,#10366,#10367);
#8759=AXIS2_PLACEMENT_3D('',#12784,#10368,#10369);
#8760=AXIS2_PLACEMENT_3D('',#12785,#10370,#10371);
#8761=AXIS2_PLACEMENT_3D('',#12787,#10372,#10373);
#8762=AXIS2_PLACEMENT_3D('',#12789,#10375,#10376);
#8763=AXIS2_PLACEMENT_3D('',#12791,#10377,#10378);
#8764=AXIS2_PLACEMENT_3D('',#12792,#10379,#10380);
#8765=AXIS2_PLACEMENT_3D('',#12794,#10382,#10383);
#8766=AXIS2_PLACEMENT_3D('',#12795,#10384,#10385);
#8767=AXIS2_PLACEMENT_3D('',#12796,#10386,#10387);
#8768=AXIS2_PLACEMENT_3D('',#12797,#10388,#10389);
#8769=AXIS2_PLACEMENT_3D('',#12799,#10390,#10391);
#8770=AXIS2_PLACEMENT_3D('',#12800,#10392,#10393);
#8771=AXIS2_PLACEMENT_3D('',#12801,#10394,#10395);
#8772=AXIS2_PLACEMENT_3D('',#12802,#10396,#10397);
#8773=AXIS2_PLACEMENT_3D('',#12804,#10398,#10399);
#8774=AXIS2_PLACEMENT_3D('',#12807,#10401,#10402);
#8775=AXIS2_PLACEMENT_3D('',#12808,#10403,#10404);
#8776=AXIS2_PLACEMENT_3D('',#12810,#10405,#10406);
#8777=AXIS2_PLACEMENT_3D('',#12811,#10407,#10408);
#8778=AXIS2_PLACEMENT_3D('',#12813,#10409,#10410);
#8779=AXIS2_PLACEMENT_3D('',#12814,#10411,#10412);
#8780=AXIS2_PLACEMENT_3D('',#12817,#10414,#10415);
#8781=AXIS2_PLACEMENT_3D('',#12818,#10416,#10417);
#8782=AXIS2_PLACEMENT_3D('',#12820,#10418,#10419);
#8783=AXIS2_PLACEMENT_3D('',#12822,#10421,#10422);
#8784=AXIS2_PLACEMENT_3D('',#12824,#10423,#10424);
#8785=AXIS2_PLACEMENT_3D('',#12827,#10426,#10427);
#8786=AXIS2_PLACEMENT_3D('',#12828,#10428,#10429);
#8787=AXIS2_PLACEMENT_3D('',#12829,#10430,#10431);
#8788=AXIS2_PLACEMENT_3D('',#12830,#10432,#10433);
#8789=AXIS2_PLACEMENT_3D('',#12831,#10434,#10435);
#8790=AXIS2_PLACEMENT_3D('',#12833,#10436,#10437);
#8791=AXIS2_PLACEMENT_3D('',#12834,#10438,#10439);
#8792=AXIS2_PLACEMENT_3D('',#12835,#10440,#10441);
#8793=AXIS2_PLACEMENT_3D('',#12836,#10442,#10443);
#8794=AXIS2_PLACEMENT_3D('',#12838,#10444,#10445);
#8795=AXIS2_PLACEMENT_3D('',#12841,#10447,#10448);
#8796=AXIS2_PLACEMENT_3D('',#12842,#10449,#10450);
#8797=AXIS2_PLACEMENT_3D('',#12843,#10451,#10452);
#8798=AXIS2_PLACEMENT_3D('',#12844,#10453,#10454);
#8799=AXIS2_PLACEMENT_3D('',#12845,#10455,#10456);
#8800=AXIS2_PLACEMENT_3D('',#12847,#10457,#10458);
#8801=AXIS2_PLACEMENT_3D('',#12850,#10460,#10461);
#8802=AXIS2_PLACEMENT_3D('',#12851,#10462,#10463);
#8803=AXIS2_PLACEMENT_3D('',#12854,#10465,#10466);
#8804=AXIS2_PLACEMENT_3D('',#12855,#10467,#10468);
#8805=AXIS2_PLACEMENT_3D('',#12857,#10469,#10470);
#8806=AXIS2_PLACEMENT_3D('',#12858,#10471,#10472);
#8807=AXIS2_PLACEMENT_3D('',#12861,#10474,#10475);
#8808=AXIS2_PLACEMENT_3D('',#12862,#10476,#10477);
#8809=AXIS2_PLACEMENT_3D('',#12863,#10478,#10479);
#8810=AXIS2_PLACEMENT_3D('',#12864,#10480,#10481);
#8811=AXIS2_PLACEMENT_3D('',#12876,#10483,#10484);
#8812=AXIS2_PLACEMENT_3D('',#12892,#10485,#10486);
#8813=AXIS2_PLACEMENT_3D('',#12894,#10487,#10488);
#8814=AXIS2_PLACEMENT_3D('',#12920,#10490,#10491);
#8815=AXIS2_PLACEMENT_3D('',#12923,#10494,#10495);
#8816=AXIS2_PLACEMENT_3D('',#12925,#10497,#10498);
#8817=AXIS2_PLACEMENT_3D('',#12927,#10500,#10501);
#8818=AXIS2_PLACEMENT_3D('',#12929,#10502,#10503);
#8819=AXIS2_PLACEMENT_3D('',#12932,#10505,#10506);
#8820=AXIS2_PLACEMENT_3D('',#12933,#10507,#10508);
#8821=AXIS2_PLACEMENT_3D('',#12935,#10510,#10511);
#8822=AXIS2_PLACEMENT_3D('',#12937,#10513,#10514);
#8823=AXIS2_PLACEMENT_3D('',#12938,#10515,#10516);
#8824=AXIS2_PLACEMENT_3D('',#12939,#10517,#10518);
#8825=AXIS2_PLACEMENT_3D('',#12940,#10519,#10520);
#8826=AXIS2_PLACEMENT_3D('',#12941,#10521,#10522);
#8827=AXIS2_PLACEMENT_3D('',#12943,#10523,#10524);
#8828=AXIS2_PLACEMENT_3D('',#12946,#10526,#10527);
#8829=AXIS2_PLACEMENT_3D('',#12947,#10528,#10529);
#8830=AXIS2_PLACEMENT_3D('',#12949,#10530,#10531);
#8831=AXIS2_PLACEMENT_3D('',#12952,#10533,#10534);
#8832=AXIS2_PLACEMENT_3D('',#12953,#10535,#10536);
#8833=AXIS2_PLACEMENT_3D('',#12955,#10537,#10538);
#8834=AXIS2_PLACEMENT_3D('',#12958,#10540,#10541);
#8835=AXIS2_PLACEMENT_3D('',#12959,#10542,#10543);
#8836=AXIS2_PLACEMENT_3D('',#12961,#10544,#10545);
#8837=AXIS2_PLACEMENT_3D('',#12964,#10547,#10548);
#8838=AXIS2_PLACEMENT_3D('',#12965,#10549,#10550);
#8839=AXIS2_PLACEMENT_3D('',#12967,#10551,#10552);
#8840=AXIS2_PLACEMENT_3D('',#12970,#10554,#10555);
#8841=AXIS2_PLACEMENT_3D('',#12971,#10556,#10557);
#8842=AXIS2_PLACEMENT_3D('',#12973,#10558,#10559);
#8843=AXIS2_PLACEMENT_3D('',#12976,#10561,#10562);
#8844=AXIS2_PLACEMENT_3D('',#12977,#10563,#10564);
#8845=AXIS2_PLACEMENT_3D('',#12979,#10565,#10566);
#8846=AXIS2_PLACEMENT_3D('',#12982,#10568,#10569);
#8847=AXIS2_PLACEMENT_3D('',#12983,#10570,#10571);
#8848=AXIS2_PLACEMENT_3D('',#12985,#10572,#10573);
#8849=AXIS2_PLACEMENT_3D('',#12988,#10575,#10576);
#8850=AXIS2_PLACEMENT_3D('',#12989,#10577,#10578);
#8851=AXIS2_PLACEMENT_3D('',#12991,#10579,#10580);
#8852=AXIS2_PLACEMENT_3D('',#12994,#10582,#10583);
#8853=AXIS2_PLACEMENT_3D('',#12995,#10584,#10585);
#8854=AXIS2_PLACEMENT_3D('',#12997,#10586,#10587);
#8855=AXIS2_PLACEMENT_3D('',#13000,#10589,#10590);
#8856=AXIS2_PLACEMENT_3D('',#13001,#10591,#10592);
#8857=AXIS2_PLACEMENT_3D('',#13003,#10593,#10594);
#8858=AXIS2_PLACEMENT_3D('',#13006,#10596,#10597);
#8859=AXIS2_PLACEMENT_3D('',#13007,#10598,#10599);
#8860=AXIS2_PLACEMENT_3D('',#13009,#10600,#10601);
#8861=AXIS2_PLACEMENT_3D('',#13012,#10603,#10604);
#8862=AXIS2_PLACEMENT_3D('',#13013,#10605,#10606);
#8863=AXIS2_PLACEMENT_3D('',#13015,#10607,#10608);
#8864=AXIS2_PLACEMENT_3D('',#13018,#10610,#10611);
#8865=AXIS2_PLACEMENT_3D('',#13019,#10612,#10613);
#8866=AXIS2_PLACEMENT_3D('',#13028,#10618,#10619);
#8867=AXIS2_PLACEMENT_3D('',#13037,#10624,#10625);
#8868=AXIS2_PLACEMENT_3D('',#13040,#10628,#10629);
#8869=AXIS2_PLACEMENT_3D('',#13042,#10631,#10632);
#8870=AXIS2_PLACEMENT_3D('',#13044,#10634,#10635);
#8871=AXIS2_PLACEMENT_3D('',#13046,#10636,#10637);
#8872=AXIS2_PLACEMENT_3D('',#13049,#10639,#10640);
#8873=AXIS2_PLACEMENT_3D('',#13050,#10641,#10642);
#8874=AXIS2_PLACEMENT_3D('',#13052,#10643,#10644);
#8875=AXIS2_PLACEMENT_3D('',#13055,#10646,#10647);
#8876=AXIS2_PLACEMENT_3D('',#13056,#10648,#10649);
#8877=AXIS2_PLACEMENT_3D('',#13058,#10650,#10651);
#8878=AXIS2_PLACEMENT_3D('',#13061,#10653,#10654);
#8879=AXIS2_PLACEMENT_3D('',#13062,#10655,#10656);
#8880=AXIS2_PLACEMENT_3D('',#13064,#10657,#10658);
#8881=AXIS2_PLACEMENT_3D('',#13067,#10660,#10661);
#8882=AXIS2_PLACEMENT_3D('',#13068,#10662,#10663);
#8883=AXIS2_PLACEMENT_3D('',#13070,#10664,#10665);
#8884=AXIS2_PLACEMENT_3D('',#13073,#10667,#10668);
#8885=AXIS2_PLACEMENT_3D('',#13074,#10669,#10670);
#8886=AXIS2_PLACEMENT_3D('',#13083,#10675,#10676);
#8887=AXIS2_PLACEMENT_3D('',#13092,#10681,#10682);
#8888=AXIS2_PLACEMENT_3D('',#13095,#10685,#10686);
#8889=AXIS2_PLACEMENT_3D('',#13097,#10688,#10689);
#8890=AXIS2_PLACEMENT_3D('',#13099,#10691,#10692);
#8891=AXIS2_PLACEMENT_3D('',#13108,#10697,#10698);
#8892=AXIS2_PLACEMENT_3D('',#13114,#10702,#10703);
#8893=AXIS2_PLACEMENT_3D('',#13120,#10707,#10708);
#8894=AXIS2_PLACEMENT_3D('',#13123,#10711,#10712);
#8895=AXIS2_PLACEMENT_3D('',#13124,#10713,#10714);
#8896=AXIS2_PLACEMENT_3D('',#13125,#10715,#10716);
#8897=AXIS2_PLACEMENT_3D('',#13126,#10717,#10718);
#8898=AXIS2_PLACEMENT_3D('',#13128,#10719,#10720);
#8899=AXIS2_PLACEMENT_3D('',#13131,#10722,#10723);
#8900=AXIS2_PLACEMENT_3D('',#13132,#10724,#10725);
#8901=AXIS2_PLACEMENT_3D('',#13134,#10726,#10727);
#8902=AXIS2_PLACEMENT_3D('',#13137,#10729,#10730);
#8903=AXIS2_PLACEMENT_3D('',#13138,#10731,#10732);
#8904=AXIS2_PLACEMENT_3D('',#13140,#10733,#10734);
#8905=AXIS2_PLACEMENT_3D('',#13143,#10736,#10737);
#8906=AXIS2_PLACEMENT_3D('',#13144,#10738,#10739);
#8907=AXIS2_PLACEMENT_3D('',#13146,#10740,#10741);
#8908=AXIS2_PLACEMENT_3D('',#13149,#10743,#10744);
#8909=AXIS2_PLACEMENT_3D('',#13150,#10745,#10746);
#8910=AXIS2_PLACEMENT_3D('',#13152,#10747,#10748);
#8911=AXIS2_PLACEMENT_3D('',#13155,#10750,#10751);
#8912=AXIS2_PLACEMENT_3D('',#13156,#10752,#10753);
#8913=AXIS2_PLACEMENT_3D('',#13158,#10754,#10755);
#8914=AXIS2_PLACEMENT_3D('',#13161,#10757,#10758);
#8915=AXIS2_PLACEMENT_3D('',#13162,#10759,#10760);
#8916=AXIS2_PLACEMENT_3D('',#13163,#10761,#10762);
#8917=AXIS2_PLACEMENT_3D('',#13164,#10763,#10764);
#8918=AXIS2_PLACEMENT_3D('',#13165,#10765,#10766);
#8919=AXIS2_PLACEMENT_3D('',#13167,#10767,#10768);
#8920=AXIS2_PLACEMENT_3D('',#13170,#10770,#10771);
#8921=AXIS2_PLACEMENT_3D('',#13171,#10772,#10773);
#8922=AXIS2_PLACEMENT_3D('',#13173,#10774,#10775);
#8923=AXIS2_PLACEMENT_3D('',#13176,#10777,#10778);
#8924=AXIS2_PLACEMENT_3D('',#13177,#10779,#10780);
#8925=AXIS2_PLACEMENT_3D('',#13179,#10781,#10782);
#8926=AXIS2_PLACEMENT_3D('',#13182,#10784,#10785);
#8927=AXIS2_PLACEMENT_3D('',#13183,#10786,#10787);
#8928=AXIS2_PLACEMENT_3D('',#13185,#10788,#10789);
#8929=AXIS2_PLACEMENT_3D('',#13188,#10791,#10792);
#8930=AXIS2_PLACEMENT_3D('',#13189,#10793,#10794);
#8931=AXIS2_PLACEMENT_3D('',#13191,#10795,#10796);
#8932=AXIS2_PLACEMENT_3D('',#13194,#10798,#10799);
#8933=AXIS2_PLACEMENT_3D('',#13195,#10800,#10801);
#8934=AXIS2_PLACEMENT_3D('',#13197,#10802,#10803);
#8935=AXIS2_PLACEMENT_3D('',#13200,#10805,#10806);
#8936=AXIS2_PLACEMENT_3D('',#13201,#10807,#10808);
#8937=AXIS2_PLACEMENT_3D('',#13202,#10809,#10810);
#8938=AXIS2_PLACEMENT_3D('',#13203,#10811,#10812);
#8939=AXIS2_PLACEMENT_3D('',#13204,#10813,#10814);
#8940=AXIS2_PLACEMENT_3D('',#13206,#10815,#10816);
#8941=AXIS2_PLACEMENT_3D('',#13209,#10818,#10819);
#8942=AXIS2_PLACEMENT_3D('',#13210,#10820,#10821);
#8943=AXIS2_PLACEMENT_3D('',#13212,#10822,#10823);
#8944=AXIS2_PLACEMENT_3D('',#13215,#10825,#10826);
#8945=AXIS2_PLACEMENT_3D('',#13216,#10827,#10828);
#8946=AXIS2_PLACEMENT_3D('',#13218,#10829,#10830);
#8947=AXIS2_PLACEMENT_3D('',#13221,#10832,#10833);
#8948=AXIS2_PLACEMENT_3D('',#13222,#10834,#10835);
#8949=AXIS2_PLACEMENT_3D('',#13224,#10836,#10837);
#8950=AXIS2_PLACEMENT_3D('',#13227,#10839,#10840);
#8951=AXIS2_PLACEMENT_3D('',#13228,#10841,#10842);
#8952=AXIS2_PLACEMENT_3D('',#13230,#10843,#10844);
#8953=AXIS2_PLACEMENT_3D('',#13233,#10846,#10847);
#8954=AXIS2_PLACEMENT_3D('',#13234,#10848,#10849);
#8955=AXIS2_PLACEMENT_3D('',#13236,#10850,#10851);
#8956=AXIS2_PLACEMENT_3D('',#13239,#10853,#10854);
#8957=AXIS2_PLACEMENT_3D('',#13240,#10855,#10856);
#8958=AXIS2_PLACEMENT_3D('',#13241,#10857,#10858);
#8959=AXIS2_PLACEMENT_3D('',#13242,#10859,#10860);
#8960=AXIS2_PLACEMENT_3D('',#13243,#10861,#10862);
#8961=AXIS2_PLACEMENT_3D('',#13245,#10863,#10864);
#8962=AXIS2_PLACEMENT_3D('',#13248,#10866,#10867);
#8963=AXIS2_PLACEMENT_3D('',#13249,#10868,#10869);
#8964=AXIS2_PLACEMENT_3D('',#13251,#10870,#10871);
#8965=AXIS2_PLACEMENT_3D('',#13254,#10873,#10874);
#8966=AXIS2_PLACEMENT_3D('',#13255,#10875,#10876);
#8967=AXIS2_PLACEMENT_3D('',#13257,#10877,#10878);
#8968=AXIS2_PLACEMENT_3D('',#13260,#10880,#10881);
#8969=AXIS2_PLACEMENT_3D('',#13261,#10882,#10883);
#8970=AXIS2_PLACEMENT_3D('',#13263,#10884,#10885);
#8971=AXIS2_PLACEMENT_3D('',#13266,#10887,#10888);
#8972=AXIS2_PLACEMENT_3D('',#13267,#10889,#10890);
#8973=AXIS2_PLACEMENT_3D('',#13269,#10891,#10892);
#8974=AXIS2_PLACEMENT_3D('',#13272,#10894,#10895);
#8975=AXIS2_PLACEMENT_3D('',#13273,#10896,#10897);
#8976=AXIS2_PLACEMENT_3D('',#13275,#10898,#10899);
#8977=AXIS2_PLACEMENT_3D('',#13278,#10901,#10902);
#8978=AXIS2_PLACEMENT_3D('',#13279,#10903,#10904);
#8979=AXIS2_PLACEMENT_3D('',#13280,#10905,#10906);
#8980=AXIS2_PLACEMENT_3D('',#13281,#10907,#10908);
#8981=AXIS2_PLACEMENT_3D('',#13282,#10909,#10910);
#8982=AXIS2_PLACEMENT_3D('',#13283,#10911,#10912);
#8983=AXIS2_PLACEMENT_3D('',#13286,#10913,#10914);
#8984=AXIS2_PLACEMENT_3D('',#13292,#10918,#10919);
#8985=AXIS2_PLACEMENT_3D('',#13298,#10923,#10924);
#8986=AXIS2_PLACEMENT_3D('',#13300,#10925,#10926);
#8987=AXIS2_PLACEMENT_3D('',#13304,#10929,#10930);
#8988=AXIS2_PLACEMENT_3D('',#13307,#10933,#10934);
#8989=AXIS2_PLACEMENT_3D('',#13308,#10935,#10936);
#8990=AXIS2_PLACEMENT_3D('',#13310,#10937,#10938);
#8991=AXIS2_PLACEMENT_3D('',#13312,#10939,#10940);
#8992=AXIS2_PLACEMENT_3D('',#13313,#10941,#10942);
#8993=AXIS2_PLACEMENT_3D('',#13315,#10943,#10944);
#8994=AXIS2_PLACEMENT_3D('',#13317,#10946,#10947);
#8995=AXIS2_PLACEMENT_3D('',#13319,#10948,#10949);
#8996=AXIS2_PLACEMENT_3D('',#13320,#10950,#10951);
#8997=AXIS2_PLACEMENT_3D('',#13322,#10952,#10953);
#8998=AXIS2_PLACEMENT_3D('',#13324,#10955,#10956);
#8999=AXIS2_PLACEMENT_3D('',#13326,#10957,#10958);
#9000=AXIS2_PLACEMENT_3D('',#13327,#10959,#10960);
#9001=AXIS2_PLACEMENT_3D('',#13329,#10961,#10962);
#9002=AXIS2_PLACEMENT_3D('',#13331,#10964,#10965);
#9003=AXIS2_PLACEMENT_3D('',#13333,#10966,#10967);
#9004=AXIS2_PLACEMENT_3D('',#13334,#10968,#10969);
#9005=AXIS2_PLACEMENT_3D('',#13336,#10970,#10971);
#9006=AXIS2_PLACEMENT_3D('',#13338,#10973,#10974);
#9007=AXIS2_PLACEMENT_3D('',#13340,#10975,#10976);
#9008=AXIS2_PLACEMENT_3D('',#13341,#10977,#10978);
#9009=AXIS2_PLACEMENT_3D('',#13343,#10979,#10980);
#9010=AXIS2_PLACEMENT_3D('',#13345,#10982,#10983);
#9011=AXIS2_PLACEMENT_3D('',#13347,#10984,#10985);
#9012=AXIS2_PLACEMENT_3D('',#13348,#10986,#10987);
#9013=AXIS2_PLACEMENT_3D('',#13350,#10989,#10990);
#9014=AXIS2_PLACEMENT_3D('',#13351,#10991,#10992);
#9015=AXIS2_PLACEMENT_3D('',#13354,#10993,#10994);
#9016=AXIS2_PLACEMENT_3D('',#13358,#10996,#10997);
#9017=AXIS2_PLACEMENT_3D('',#13360,#10999,#11000);
#9018=AXIS2_PLACEMENT_3D('',#13366,#11004,#11005);
#9019=AXIS2_PLACEMENT_3D('',#13368,#11006,#11007);
#9020=AXIS2_PLACEMENT_3D('',#13370,#11008,#11009);
#9021=AXIS2_PLACEMENT_3D('',#13372,#11011,#11012);
#9022=AXIS2_PLACEMENT_3D('',#13375,#11015,#11016);
#9023=AXIS2_PLACEMENT_3D('',#13377,#11017,#11018);
#9024=AXIS2_PLACEMENT_3D('',#13379,#11019,#11020);
#9025=AXIS2_PLACEMENT_3D('',#13380,#11021,#11022);
#9026=AXIS2_PLACEMENT_3D('',#13382,#11023,#11024);
#9027=AXIS2_PLACEMENT_3D('',#13384,#11026,#11027);
#9028=AXIS2_PLACEMENT_3D('',#13386,#11028,#11029);
#9029=AXIS2_PLACEMENT_3D('',#13387,#11030,#11031);
#9030=AXIS2_PLACEMENT_3D('',#13389,#11033,#11034);
#9031=AXIS2_PLACEMENT_3D('',#13390,#11035,#11036);
#9032=AXIS2_PLACEMENT_3D('',#13391,#11037,#11038);
#9033=AXIS2_PLACEMENT_3D('',#13392,#11039,#11040);
#9034=AXIS2_PLACEMENT_3D('',#13401,#11045,#11046);
#9035=AXIS2_PLACEMENT_3D('',#13407,#11050,#11051);
#9036=AXIS2_PLACEMENT_3D('',#13413,#11055,#11056);
#9037=AXIS2_PLACEMENT_3D('',#13419,#11060,#11061);
#9038=AXIS2_PLACEMENT_3D('',#13425,#11065,#11066);
#9039=AXIS2_PLACEMENT_3D('',#13428,#11069,#11070);
#9040=AXIS2_PLACEMENT_3D('',#13429,#11071,#11072);
#9041=AXIS2_PLACEMENT_3D('',#13430,#11073,#11074);
#9042=AXIS2_PLACEMENT_3D('',#13432,#11075,#11076);
#9043=AXIS2_PLACEMENT_3D('',#13433,#11077,#11078);
#9044=AXIS2_PLACEMENT_3D('',#13435,#11079,#11080);
#9045=AXIS2_PLACEMENT_3D('',#13436,#11081,#11082);
#9046=AXIS2_PLACEMENT_3D('',#13438,#11083,#11084);
#9047=AXIS2_PLACEMENT_3D('',#13440,#11086,#11087);
#9048=AXIS2_PLACEMENT_3D('',#13442,#11088,#11089);
#9049=AXIS2_PLACEMENT_3D('',#13444,#11091,#11092);
#9050=AXIS2_PLACEMENT_3D('',#13446,#11093,#11094);
#9051=AXIS2_PLACEMENT_3D('',#13448,#11096,#11097);
#9052=AXIS2_PLACEMENT_3D('',#13450,#11098,#11099);
#9053=AXIS2_PLACEMENT_3D('',#13451,#11100,#11101);
#9054=AXIS2_PLACEMENT_3D('',#13453,#11102,#11103);
#9055=AXIS2_PLACEMENT_3D('',#13455,#11105,#11106);
#9056=AXIS2_PLACEMENT_3D('',#13457,#11108,#11109);
#9057=AXIS2_PLACEMENT_3D('',#13458,#11110,#11111);
#9058=AXIS2_PLACEMENT_3D('',#13467,#11116,#11117);
#9059=AXIS2_PLACEMENT_3D('',#13473,#11121,#11122);
#9060=AXIS2_PLACEMENT_3D('',#13479,#11126,#11127);
#9061=AXIS2_PLACEMENT_3D('',#13485,#11131,#11132);
#9062=AXIS2_PLACEMENT_3D('',#13491,#11136,#11137);
#9063=AXIS2_PLACEMENT_3D('',#13494,#11140,#11141);
#9064=AXIS2_PLACEMENT_3D('',#13495,#11142,#11143);
#9065=AXIS2_PLACEMENT_3D('',#13496,#11144,#11145);
#9066=AXIS2_PLACEMENT_3D('',#13498,#11146,#11147);
#9067=AXIS2_PLACEMENT_3D('',#13500,#11148,#11149);
#9068=AXIS2_PLACEMENT_3D('',#13501,#11150,#11151);
#9069=AXIS2_PLACEMENT_3D('',#13504,#11153,#11154);
#9070=AXIS2_PLACEMENT_3D('',#13505,#11155,#11156);
#9071=AXIS2_PLACEMENT_3D('',#13506,#11157,#11158);
#9072=AXIS2_PLACEMENT_3D('',#13508,#11159,#11160);
#9073=AXIS2_PLACEMENT_3D('',#13509,#11161,#11162);
#9074=AXIS2_PLACEMENT_3D('',#13511,#11163,#11164);
#9075=AXIS2_PLACEMENT_3D('',#13513,#11166,#11167);
#9076=AXIS2_PLACEMENT_3D('',#13515,#11168,#11169);
#9077=AXIS2_PLACEMENT_3D('',#13517,#11171,#11172);
#9078=AXIS2_PLACEMENT_3D('',#13519,#11173,#11174);
#9079=AXIS2_PLACEMENT_3D('',#13521,#11176,#11177);
#9080=AXIS2_PLACEMENT_3D('',#13523,#11178,#11179);
#9081=AXIS2_PLACEMENT_3D('',#13524,#11180,#11181);
#9082=AXIS2_PLACEMENT_3D('',#13526,#11182,#11183);
#9083=AXIS2_PLACEMENT_3D('',#13528,#11185,#11186);
#9084=AXIS2_PLACEMENT_3D('',#13530,#11187,#11188);
#9085=AXIS2_PLACEMENT_3D('',#13532,#11190,#11191);
#9086=AXIS2_PLACEMENT_3D('',#13534,#11193,#11194);
#9087=AXIS2_PLACEMENT_3D('',#13535,#11195,#11196);
#9088=AXIS2_PLACEMENT_3D('',#13536,#11197,#11198);
#9089=AXIS2_PLACEMENT_3D('',#13537,#11199,#11200);
#9090=AXIS2_PLACEMENT_3D('',#13538,#11201,#11202);
#9091=AXIS2_PLACEMENT_3D('',#13539,#11203,#11204);
#9092=AXIS2_PLACEMENT_3D('',#13540,#11205,#11206);
#9093=AXIS2_PLACEMENT_3D('',#13541,#11207,#11208);
#9094=AXIS2_PLACEMENT_3D('',#13542,#11209,#11210);
#9095=AXIS2_PLACEMENT_3D('',#13543,#11211,#11212);
#9096=AXIS2_PLACEMENT_3D('',#13544,#11213,#11214);
#9097=AXIS2_PLACEMENT_3D('',#13545,#11215,#11216);
#9098=AXIS2_PLACEMENT_3D('',#13546,#11217,#11218);
#9099=AXIS2_PLACEMENT_3D('',#13547,#11219,#11220);
#9100=AXIS2_PLACEMENT_3D('',#13548,#11221,#11222);
#9101=AXIS2_PLACEMENT_3D('',#13549,#11223,#11224);
#9102=AXIS2_PLACEMENT_3D('',#13550,#11225,#11226);
#9103=AXIS2_PLACEMENT_3D('',#13551,#11227,#11228);
#9104=AXIS2_PLACEMENT_3D('',#13552,#11229,#11230);
#9105=AXIS2_PLACEMENT_3D('',#13553,#11231,#11232);
#9106=AXIS2_PLACEMENT_3D('',#13554,#11233,#11234);
#9107=AXIS2_PLACEMENT_3D('',#13555,#11235,#11236);
#9108=AXIS2_PLACEMENT_3D('',#13556,#11237,#11238);
#9109=AXIS2_PLACEMENT_3D('',#13557,#11239,#11240);
#9110=AXIS2_PLACEMENT_3D('',#13558,#11241,#11242);
#9111=AXIS2_PLACEMENT_3D('',#13559,#11243,#11244);
#9112=AXIS2_PLACEMENT_3D('',#13560,#11245,#11246);
#9113=AXIS2_PLACEMENT_3D('',#13561,#11247,#11248);
#9114=AXIS2_PLACEMENT_3D('',#13562,#11249,#11250);
#9115=AXIS2_PLACEMENT_3D('',#13563,#11251,#11252);
#9116=AXIS2_PLACEMENT_3D('',#13564,#11253,#11254);
#9117=AXIS2_PLACEMENT_3D('',#13565,#11255,#11256);
#9118=AXIS2_PLACEMENT_3D('',#13566,#11257,#11258);
#9119=AXIS2_PLACEMENT_3D('',#13567,#11259,#11260);
#9120=AXIS2_PLACEMENT_3D('',#13568,#11261,#11262);
#9121=AXIS2_PLACEMENT_3D('',#13569,#11263,#11264);
#9122=AXIS2_PLACEMENT_3D('',#13570,#11265,#11266);
#9123=AXIS2_PLACEMENT_3D('',#13571,#11267,#11268);
#9124=AXIS2_PLACEMENT_3D('',#13572,#11269,#11270);
#9125=AXIS2_PLACEMENT_3D('',#13573,#11271,#11272);
#9126=AXIS2_PLACEMENT_3D('',#13574,#11273,#11274);
#9127=AXIS2_PLACEMENT_3D('',#13575,#11275,#11276);
#9128=AXIS2_PLACEMENT_3D('',#13576,#11277,#11278);
#9129=AXIS2_PLACEMENT_3D('',#13577,#11279,#11280);
#9130=AXIS2_PLACEMENT_3D('',#13578,#11281,#11282);
#9131=AXIS2_PLACEMENT_3D('',#13579,#11283,#11284);
#9132=AXIS2_PLACEMENT_3D('',#13580,#11285,#11286);
#9133=AXIS2_PLACEMENT_3D('',#13581,#11287,#11288);
#9134=AXIS2_PLACEMENT_3D('',#13582,#11289,#11290);
#9135=AXIS2_PLACEMENT_3D('',#13583,#11291,#11292);
#9136=AXIS2_PLACEMENT_3D('',#13584,#11293,#11294);
#9137=AXIS2_PLACEMENT_3D('',#13585,#11295,#11296);
#9138=AXIS2_PLACEMENT_3D('',#13586,#11297,#11298);
#9139=AXIS2_PLACEMENT_3D('',#13587,#11299,#11300);
#9140=AXIS2_PLACEMENT_3D('',#13588,#11301,#11302);
#9141=AXIS2_PLACEMENT_3D('',#13589,#11303,#11304);
#9142=AXIS2_PLACEMENT_3D('',#13590,#11305,#11306);
#9143=AXIS2_PLACEMENT_3D('',#13591,#11307,#11308);
#9144=AXIS2_PLACEMENT_3D('',#13592,#11309,#11310);
#9145=AXIS2_PLACEMENT_3D('',#13593,#11311,#11312);
#9146=AXIS2_PLACEMENT_3D('',#13594,#11313,#11314);
#9147=AXIS2_PLACEMENT_3D('',#13595,#11315,#11316);
#9148=AXIS2_PLACEMENT_3D('',#13596,#11317,#11318);
#9149=AXIS2_PLACEMENT_3D('',#13597,#11319,#11320);
#9150=AXIS2_PLACEMENT_3D('',#13598,#11321,#11322);
#9151=AXIS2_PLACEMENT_3D('',#13599,#11323,#11324);
#9152=AXIS2_PLACEMENT_3D('',#13600,#11325,#11326);
#9153=AXIS2_PLACEMENT_3D('',#13601,#11327,#11328);
#9154=AXIS2_PLACEMENT_3D('',#13602,#11329,#11330);
#9155=AXIS2_PLACEMENT_3D('',#13603,#11331,#11332);
#9156=AXIS2_PLACEMENT_3D('',#13604,#11333,#11334);
#9157=AXIS2_PLACEMENT_3D('',#13606,#11335,#11336);
#9158=AXIS2_PLACEMENT_3D('',#13609,#11338,#11339);
#9159=AXIS2_PLACEMENT_3D('',#13610,#11340,#11341);
#9160=AXIS2_PLACEMENT_3D('',#13612,#11342,#11343);
#9161=AXIS2_PLACEMENT_3D('',#13613,#11344,#11345);
#9162=AXIS2_PLACEMENT_3D('',#13615,#11346,#11347);
#9163=AXIS2_PLACEMENT_3D('',#13618,#11349,#11350);
#9164=AXIS2_PLACEMENT_3D('',#13619,#11351,#11352);
#9165=AXIS2_PLACEMENT_3D('',#13621,#11353,#11354);
#9166=AXIS2_PLACEMENT_3D('',#13622,#11355,#11356);
#9167=AXIS2_PLACEMENT_3D('',#13624,#11357,#11358);
#9168=AXIS2_PLACEMENT_3D('',#13625,#11359,#11360);
#9169=AXIS2_PLACEMENT_3D('',#13628,#11362,#11363);
#9170=AXIS2_PLACEMENT_3D('',#13629,#11364,#11365);
#9171=AXIS2_PLACEMENT_3D('',#13632,#11367,#11368);
#9172=AXIS2_PLACEMENT_3D('',#13633,#11369,#11370);
#9173=AXIS2_PLACEMENT_3D('',#13635,#11371,#11372);
#9174=AXIS2_PLACEMENT_3D('',#13637,#11374,#11375);
#9175=AXIS2_PLACEMENT_3D('',#13638,#11376,#11377);
#9176=AXIS2_PLACEMENT_3D('',#13639,#11378,#11379);
#9177=AXIS2_PLACEMENT_3D('',#13640,#11380,#11381);
#9178=AXIS2_PLACEMENT_3D('',#13642,#11382,#11383);
#9179=AXIS2_PLACEMENT_3D('',#13643,#11384,#11385);
#9180=AXIS2_PLACEMENT_3D('',#13644,#11386,#11387);
#9181=AXIS2_PLACEMENT_3D('',#13645,#11388,#11389);
#9182=AXIS2_PLACEMENT_3D('',#13647,#11390,#11391);
#9183=AXIS2_PLACEMENT_3D('',#13650,#11393,#11394);
#9184=AXIS2_PLACEMENT_3D('',#13651,#11395,#11396);
#9185=AXIS2_PLACEMENT_3D('',#13652,#11397,#11398);
#9186=AXIS2_PLACEMENT_3D('',#13654,#11399,#11400);
#9187=AXIS2_PLACEMENT_3D('',#13657,#11402,#11403);
#9188=AXIS2_PLACEMENT_3D('',#13658,#11404,#11405);
#9189=AXIS2_PLACEMENT_3D('',#13659,#11406,#11407);
#9190=AXIS2_PLACEMENT_3D('',#13660,#11408,#11409);
#9191=AXIS2_PLACEMENT_3D('',#13661,#11410,#11411);
#9192=AXIS2_PLACEMENT_3D('',#13663,#11412,#11413);
#9193=AXIS2_PLACEMENT_3D('',#13664,#11414,#11415);
#9194=AXIS2_PLACEMENT_3D('',#13666,#11416,#11417);
#9195=AXIS2_PLACEMENT_3D('',#13668,#11419,#11420);
#9196=AXIS2_PLACEMENT_3D('',#13670,#11421,#11422);
#9197=AXIS2_PLACEMENT_3D('',#13672,#11424,#11425);
#9198=AXIS2_PLACEMENT_3D('',#13674,#11426,#11427);
#9199=AXIS2_PLACEMENT_3D('',#13676,#11429,#11430);
#9200=AXIS2_PLACEMENT_3D('',#13678,#11431,#11432);
#9201=AXIS2_PLACEMENT_3D('',#13679,#11433,#11434);
#9202=AXIS2_PLACEMENT_3D('',#13681,#11435,#11436);
#9203=AXIS2_PLACEMENT_3D('',#13683,#11438,#11439);
#9204=AXIS2_PLACEMENT_3D('',#13685,#11440,#11441);
#9205=AXIS2_PLACEMENT_3D('',#13687,#11443,#11444);
#9206=AXIS2_PLACEMENT_3D('',#13689,#11445,#11446);
#9207=AXIS2_PLACEMENT_3D('',#13691,#11448,#11449);
#9208=AXIS2_PLACEMENT_3D('',#13692,#11450,#11451);
#9209=AXIS2_PLACEMENT_3D('',#13701,#11456,#11457);
#9210=AXIS2_PLACEMENT_3D('',#13707,#11461,#11462);
#9211=AXIS2_PLACEMENT_3D('',#13713,#11466,#11467);
#9212=AXIS2_PLACEMENT_3D('',#13719,#11471,#11472);
#9213=AXIS2_PLACEMENT_3D('',#13725,#11476,#11477);
#9214=AXIS2_PLACEMENT_3D('',#13728,#11480,#11481);
#9215=AXIS2_PLACEMENT_3D('',#13729,#11482,#11483);
#9216=AXIS2_PLACEMENT_3D('',#13730,#11484,#11485);
#9217=AXIS2_PLACEMENT_3D('',#13731,#11486,#11487);
#9218=AXIS2_PLACEMENT_3D('',#13733,#11488,#11489);
#9219=AXIS2_PLACEMENT_3D('',#13736,#11491,#11492);
#9220=AXIS2_PLACEMENT_3D('',#13737,#11493,#11494);
#9221=AXIS2_PLACEMENT_3D('',#13739,#11495,#11496);
#9222=AXIS2_PLACEMENT_3D('',#13742,#11498,#11499);
#9223=AXIS2_PLACEMENT_3D('',#13743,#11500,#11501);
#9224=AXIS2_PLACEMENT_3D('',#13747,#11503,#11504);
#9225=AXIS2_PLACEMENT_3D('',#13748,#11505,#11506);
#9226=AXIS2_PLACEMENT_3D('',#13761,#11507,#11508);
#9227=AXIS2_PLACEMENT_3D('',#13764,#11510,#11511);
#9228=AXIS2_PLACEMENT_3D('',#13766,#11512,#11513);
#9229=AXIS2_PLACEMENT_3D('',#13777,#11514,#11515);
#9230=AXIS2_PLACEMENT_3D('',#13779,#11517,#11518);
#9231=AXIS2_PLACEMENT_3D('',#13781,#11519,#11520);
#9232=AXIS2_PLACEMENT_3D('',#13784,#11522,#11523);
#9233=AXIS2_PLACEMENT_3D('',#13785,#11524,#11525);
#9234=AXIS2_PLACEMENT_3D('',#13794,#11530,#11531);
#9235=AXIS2_PLACEMENT_3D('',#13800,#11535,#11536);
#9236=AXIS2_PLACEMENT_3D('',#13806,#11540,#11541);
#9237=AXIS2_PLACEMENT_3D('',#13816,#11547,#11548);
#9238=AXIS2_PLACEMENT_3D('',#13820,#11551,#11552);
#9239=AXIS2_PLACEMENT_3D('',#13824,#11555,#11556);
#9240=AXIS2_PLACEMENT_3D('',#13830,#11560,#11561);
#9241=AXIS2_PLACEMENT_3D('',#13832,#11563,#11564);
#9242=AXIS2_PLACEMENT_3D('',#13834,#11566,#11567);
#9243=AXIS2_PLACEMENT_3D('',#13835,#11568,#11569);
#9244=AXIS2_PLACEMENT_3D('',#13836,#11570,#11571);
#9245=AXIS2_PLACEMENT_3D('',#13845,#11576,#11577);
#9246=AXIS2_PLACEMENT_3D('',#13851,#11581,#11582);
#9247=AXIS2_PLACEMENT_3D('',#13857,#11586,#11587);
#9248=AXIS2_PLACEMENT_3D('',#13863,#11591,#11592);
#9249=AXIS2_PLACEMENT_3D('',#13869,#11596,#11597);
#9250=AXIS2_PLACEMENT_3D('',#13872,#11600,#11601);
#9251=AXIS2_PLACEMENT_3D('',#13873,#11602,#11603);
#9252=AXIS2_PLACEMENT_3D('',#13875,#11604,#11605);
#9253=AXIS2_PLACEMENT_3D('',#13876,#11606,#11607);
#9254=AXIS2_PLACEMENT_3D('',#13878,#11608,#11609);
#9255=AXIS2_PLACEMENT_3D('',#13880,#11611,#11612);
#9256=AXIS2_PLACEMENT_3D('',#13882,#11613,#11614);
#9257=AXIS2_PLACEMENT_3D('',#13884,#11616,#11617);
#9258=AXIS2_PLACEMENT_3D('',#13886,#11618,#11619);
#9259=AXIS2_PLACEMENT_3D('',#13888,#11621,#11622);
#9260=AXIS2_PLACEMENT_3D('',#13889,#11623,#11624);
#9261=AXIS2_PLACEMENT_3D('',#13890,#11625,#11626);
#9262=AXIS2_PLACEMENT_3D('',#13968,#11628,#11629);
#9263=AXIS2_PLACEMENT_3D('',#13970,#11630,#11631);
#9264=AXIS2_PLACEMENT_3D('',#13971,#11632,#11633);
#9265=AXIS2_PLACEMENT_3D('',#13973,#11634,#11635);
#9266=AXIS2_PLACEMENT_3D('',#13975,#11637,#11638);
#9267=AXIS2_PLACEMENT_3D('',#13977,#11639,#11640);
#9268=AXIS2_PLACEMENT_3D('',#13979,#11642,#11643);
#9269=AXIS2_PLACEMENT_3D('',#13981,#11644,#11645);
#9270=AXIS2_PLACEMENT_3D('',#13982,#11646,#11647);
#9271=AXIS2_PLACEMENT_3D('',#13984,#11648,#11649);
#9272=AXIS2_PLACEMENT_3D('',#13987,#11652,#11653);
#9273=AXIS2_PLACEMENT_3D('',#13989,#11654,#11655);
#9274=AXIS2_PLACEMENT_3D('',#13991,#11657,#11658);
#9275=AXIS2_PLACEMENT_3D('',#13992,#11659,#11660);
#9276=AXIS2_PLACEMENT_3D('',#13993,#11661,#11662);
#9277=AXIS2_PLACEMENT_3D('',#13995,#11663,#11664);
#9278=AXIS2_PLACEMENT_3D('',#13998,#11666,#11667);
#9279=AXIS2_PLACEMENT_3D('',#13999,#11668,#11669);
#9280=AXIS2_PLACEMENT_3D('',#14001,#11670,#11671);
#9281=AXIS2_PLACEMENT_3D('',#14004,#11673,#11674);
#9282=AXIS2_PLACEMENT_3D('',#14005,#11675,#11676);
#9283=AXIS2_PLACEMENT_3D('',#14006,#11677,#11678);
#9284=AXIS2_PLACEMENT_3D('',#14007,#11679,#11680);
#9285=AXIS2_PLACEMENT_3D('',#14008,#11681,#11682);
#9286=AXIS2_PLACEMENT_3D('',#14010,#11683,#11684);
#9287=AXIS2_PLACEMENT_3D('',#14011,#11685,#11686);
#9288=AXIS2_PLACEMENT_3D('',#14066,#11687,#11688);
#9289=AXIS2_PLACEMENT_3D('',#14069,#11689,#11690);
#9290=AXIS2_PLACEMENT_3D('',#14071,#11692,#11693);
#9291=AXIS2_PLACEMENT_3D('',#14077,#11697,#11698);
#9292=AXIS2_PLACEMENT_3D('',#14079,#11699,#11700);
#9293=AXIS2_PLACEMENT_3D('',#14081,#11702,#11703);
#9294=AXIS2_PLACEMENT_3D('',#14082,#11704,#11705);
#9295=AXIS2_PLACEMENT_3D('',#14083,#11706,#11707);
#9296=AXIS2_PLACEMENT_3D('',#14084,#11708,#11709);
#9297=AXIS2_PLACEMENT_3D('',#14086,#11710,#11711);
#9298=AXIS2_PLACEMENT_3D('',#14089,#11713,#11714);
#9299=AXIS2_PLACEMENT_3D('',#14090,#11715,#11716);
#9300=AXIS2_PLACEMENT_3D('',#14091,#11717,#11718);
#9301=AXIS2_PLACEMENT_3D('',#14093,#11719,#11720);
#9302=AXIS2_PLACEMENT_3D('',#14096,#11722,#11723);
#9303=AXIS2_PLACEMENT_3D('',#14097,#11724,#11725);
#9304=AXIS2_PLACEMENT_3D('',#14098,#11726,#11727);
#9305=AXIS2_PLACEMENT_3D('',#14099,#11728,#11729);
#9306=AXIS2_PLACEMENT_3D('',#14100,#11730,#11731);
#9307=AXIS2_PLACEMENT_3D('',#14102,#11732,#11733);
#9308=AXIS2_PLACEMENT_3D('',#14105,#11735,#11736);
#9309=AXIS2_PLACEMENT_3D('',#14106,#11737,#11738);
#9310=AXIS2_PLACEMENT_3D('',#14107,#11739,#11740);
#9311=AXIS2_PLACEMENT_3D('',#14109,#11741,#11742);
#9312=AXIS2_PLACEMENT_3D('',#14112,#11744,#11745);
#9313=AXIS2_PLACEMENT_3D('',#14113,#11746,#11747);
#9314=AXIS2_PLACEMENT_3D('',#14114,#11748,#11749);
#9315=AXIS2_PLACEMENT_3D('',#14115,#11750,#11751);
#9316=AXIS2_PLACEMENT_3D('',#14116,#11752,#11753);
#9317=AXIS2_PLACEMENT_3D('',#14118,#11754,#11755);
#9318=AXIS2_PLACEMENT_3D('',#14121,#11757,#11758);
#9319=AXIS2_PLACEMENT_3D('',#14122,#11759,#11760);
#9320=AXIS2_PLACEMENT_3D('',#14124,#11761,#11762);
#9321=AXIS2_PLACEMENT_3D('',#14127,#11764,#11765);
#9322=AXIS2_PLACEMENT_3D('',#14128,#11766,#11767);
#9323=AXIS2_PLACEMENT_3D('',#14130,#11768,#11769);
#9324=AXIS2_PLACEMENT_3D('',#14133,#11771,#11772);
#9325=AXIS2_PLACEMENT_3D('',#14134,#11773,#11774);
#9326=AXIS2_PLACEMENT_3D('',#14143,#11779,#11780);
#9327=AXIS2_PLACEMENT_3D('',#14149,#11784,#11785);
#9328=AXIS2_PLACEMENT_3D('',#14153,#11788,#11789);
#9329=AXIS2_PLACEMENT_3D('',#14157,#11792,#11793);
#9330=AXIS2_PLACEMENT_3D('',#14159,#11795,#11796);
#9331=AXIS2_PLACEMENT_3D('',#14168,#11801,#11802);
#9332=AXIS2_PLACEMENT_3D('',#14174,#11806,#11807);
#9333=AXIS2_PLACEMENT_3D('',#14180,#11811,#11812);
#9334=AXIS2_PLACEMENT_3D('',#14183,#11815,#11816);
#9335=AXIS2_PLACEMENT_3D('',#14184,#11817,#11818);
#9336=AXIS2_PLACEMENT_3D('',#14185,#11819,#11820);
#9337=AXIS2_PLACEMENT_3D('',#14186,#11821,#11822);
#9338=AXIS2_PLACEMENT_3D('',#14188,#11823,#11824);
#9339=AXIS2_PLACEMENT_3D('',#14191,#11826,#11827);
#9340=AXIS2_PLACEMENT_3D('',#14192,#11828,#11829);
#9341=AXIS2_PLACEMENT_3D('',#14194,#11830,#11831);
#9342=AXIS2_PLACEMENT_3D('',#14197,#11833,#11834);
#9343=AXIS2_PLACEMENT_3D('',#14198,#11835,#11836);
#9344=AXIS2_PLACEMENT_3D('',#14199,#11837,#11838);
#9345=AXIS2_PLACEMENT_3D('',#14200,#11839,#11840);
#9346=AXIS2_PLACEMENT_3D('',#14201,#11841,#11842);
#9347=AXIS2_PLACEMENT_3D('',#14213,#11844,#11845);
#9348=AXIS2_PLACEMENT_3D('',#14229,#11846,#11847);
#9349=AXIS2_PLACEMENT_3D('',#14231,#11848,#11849);
#9350=AXIS2_PLACEMENT_3D('',#14257,#11851,#11852);
#9351=AXIS2_PLACEMENT_3D('',#14260,#11855,#11856);
#9352=AXIS2_PLACEMENT_3D('',#14262,#11858,#11859);
#9353=AXIS2_PLACEMENT_3D('',#14264,#11861,#11862);
#9354=AXIS2_PLACEMENT_3D('',#14266,#11863,#11864);
#9355=AXIS2_PLACEMENT_3D('',#14269,#11866,#11867);
#9356=AXIS2_PLACEMENT_3D('',#14270,#11868,#11869);
#9357=AXIS2_PLACEMENT_3D('',#14272,#11871,#11872);
#9358=AXIS2_PLACEMENT_3D('',#14274,#11874,#11875);
#9359=AXIS2_PLACEMENT_3D('',#14275,#11876,#11877);
#9360=AXIS2_PLACEMENT_3D('',#14276,#11878,#11879);
#9361=AXIS2_PLACEMENT_3D('',#14277,#11880,#11881);
#9362=AXIS2_PLACEMENT_3D('',#14278,#11882,#11883);
#9363=AXIS2_PLACEMENT_3D('',#14279,#11884,#11885);
#9364=AXIS2_PLACEMENT_3D('',#14280,#11886,#11887);
#9365=AXIS2_PLACEMENT_3D('',#14281,#11888,#11889);
#9366=AXIS2_PLACEMENT_3D('',#14282,#11890,#11891);
#9367=AXIS2_PLACEMENT_3D('',#14283,#11892,#11893);
#9368=AXIS2_PLACEMENT_3D('',#14284,#11894,#11895);
#9369=AXIS2_PLACEMENT_3D('',#14285,#11896,#11897);
#9370=AXIS2_PLACEMENT_3D('',#14286,#11898,#11899);
#9371=AXIS2_PLACEMENT_3D('',#14287,#11900,#11901);
#9372=AXIS2_PLACEMENT_3D('',#14288,#11902,#11903);
#9373=AXIS2_PLACEMENT_3D('',#14289,#11904,#11905);
#9374=AXIS2_PLACEMENT_3D('',#14290,#11906,#11907);
#9375=AXIS2_PLACEMENT_3D('',#14291,#11908,#11909);
#9376=AXIS2_PLACEMENT_3D('',#14292,#11910,#11911);
#9377=AXIS2_PLACEMENT_3D('',#14293,#11912,#11913);
#9378=AXIS2_PLACEMENT_3D('',#14294,#11914,#11915);
#9379=AXIS2_PLACEMENT_3D('',#14295,#11916,#11917);
#9380=AXIS2_PLACEMENT_3D('',#14296,#11918,#11919);
#9381=DIRECTION('axis',(0.,0.,1.));
#9382=DIRECTION('refdir',(1.,0.,0.));
#9383=DIRECTION('axis',(0.,0.,1.));
#9384=DIRECTION('refdir',(1.,0.,0.));
#9385=DIRECTION('axis',(0.,0.,1.));
#9386=DIRECTION('refdir',(1.,0.,0.));
#9387=DIRECTION('center_axis',(0.,0.,1.));
#9388=DIRECTION('ref_axis',(1.,0.,0.));
#9389=DIRECTION('center_axis',(0.,0.,1.));
#9390=DIRECTION('ref_axis',(1.,0.,0.));
#9391=DIRECTION('',(0.,0.,1.));
#9392=DIRECTION('center_axis',(0.,0.,1.));
#9393=DIRECTION('ref_axis',(1.,0.,0.));
#9394=DIRECTION('center_axis',(0.,0.,1.));
#9395=DIRECTION('ref_axis',(1.,0.,0.));
#9396=DIRECTION('center_axis',(0.,0.,1.));
#9397=DIRECTION('ref_axis',(1.,0.,0.));
#9398=DIRECTION('center_axis',(0.,0.,1.));
#9399=DIRECTION('ref_axis',(1.,0.,0.));
#9400=DIRECTION('',(0.,0.,1.));
#9401=DIRECTION('center_axis',(0.,0.,1.));
#9402=DIRECTION('ref_axis',(1.,0.,0.));
#9403=DIRECTION('center_axis',(0.,0.,1.));
#9404=DIRECTION('ref_axis',(1.,0.,0.));
#9405=DIRECTION('center_axis',(0.,1.,0.));
#9406=DIRECTION('ref_axis',(1.,0.,0.));
#9407=DIRECTION('',(-1.,0.,0.));
#9408=DIRECTION('center_axis',(0.,1.,0.));
#9409=DIRECTION('ref_axis',(1.,0.,0.));
#9410=DIRECTION('center_axis',(0.,1.,0.));
#9411=DIRECTION('ref_axis',(1.,0.,0.));
#9412=DIRECTION('',(0.,0.,-1.));
#9413=DIRECTION('center_axis',(0.,1.,0.));
#9414=DIRECTION('ref_axis',(1.,0.,0.));
#9415=DIRECTION('center_axis',(0.,1.,0.));
#9416=DIRECTION('ref_axis',(1.,0.,0.));
#9417=DIRECTION('center_axis',(0.,-0.707106781186548,-0.707106781186547));
#9418=DIRECTION('ref_axis',(0.,0.707106781186547,-0.707106781186548));
#9419=DIRECTION('center_axis',(0.,-0.707106781186548,0.707106781186547));
#9420=DIRECTION('ref_axis',(0.,-0.707106781186547,-0.707106781186548));
#9421=DIRECTION('center_axis',(0.,1.,0.));
#9422=DIRECTION('ref_axis',(1.,0.,0.));
#9423=DIRECTION('',(0.,1.,0.));
#9424=DIRECTION('',(0.,-1.,0.));
#9425=DIRECTION('center_axis',(0.,0.707106781186548,0.707106781186547));
#9426=DIRECTION('ref_axis',(0.,0.707106781186547,-0.707106781186548));
#9427=DIRECTION('center_axis',(0.,0.707106781186548,-0.707106781186547));
#9428=DIRECTION('ref_axis',(0.,-0.707106781186547,-0.707106781186548));
#9429=DIRECTION('',(0.,1.,0.));
#9430=DIRECTION('center_axis',(0.,-1.,0.));
#9431=DIRECTION('ref_axis',(1.,0.,0.));
#9432=DIRECTION('',(0.,-1.,0.));
#9433=DIRECTION('center_axis',(0.,1.,0.));
#9434=DIRECTION('ref_axis',(1.,0.,0.));
#9435=DIRECTION('',(0.,1.,0.));
#9436=DIRECTION('center_axis',(0.,-1.,0.));
#9437=DIRECTION('ref_axis',(1.,0.,0.));
#9438=DIRECTION('center_axis',(0.,0.707106781186548,0.707106781186547));
#9439=DIRECTION('ref_axis',(0.,0.707106781186547,-0.707106781186548));
#9440=DIRECTION('center_axis',(0.,1.,0.));
#9441=DIRECTION('ref_axis',(-1.,0.,-2.54207057918564E-15));
#9442=DIRECTION('center_axis',(0.,-0.707106781186548,-0.707106781186547));
#9443=DIRECTION('ref_axis',(0.,0.707106781186547,-0.707106781186548));
#9444=DIRECTION('center_axis',(0.,1.,0.));
#9445=DIRECTION('ref_axis',(1.,0.,0.));
#9446=DIRECTION('center_axis',(0.,-0.707106781186548,0.707106781186547));
#9447=DIRECTION('ref_axis',(0.,-0.707106781186547,-0.707106781186548));
#9448=DIRECTION('center_axis',(0.,1.,0.));
#9449=DIRECTION('ref_axis',(1.,0.,0.));
#9450=DIRECTION('center_axis',(0.,-1.,0.));
#9451=DIRECTION('ref_axis',(1.,0.,0.));
#9452=DIRECTION('center_axis',(0.,1.,0.));
#9453=DIRECTION('ref_axis',(1.,0.,0.));
#9454=DIRECTION('',(0.,0.,1.));
#9455=DIRECTION('center_axis',(0.,0.,1.));
#9456=DIRECTION('ref_axis',(1.,0.,0.));
#9457=DIRECTION('center_axis',(0.,0.,1.));
#9458=DIRECTION('ref_axis',(1.,0.,0.));
#9459=DIRECTION('center_axis',(0.,0.,1.));
#9460=DIRECTION('ref_axis',(1.,0.,0.));
#9461=DIRECTION('center_axis',(0.,0.,1.));
#9462=DIRECTION('ref_axis',(1.,0.,0.));
#9463=DIRECTION('center_axis',(0.,0.,1.));
#9464=DIRECTION('ref_axis',(1.,0.,0.));
#9465=DIRECTION('center_axis',(0.,0.,1.));
#9466=DIRECTION('ref_axis',(1.,0.,0.));
#9467=DIRECTION('',(0.,0.,1.));
#9468=DIRECTION('center_axis',(0.,0.,-1.));
#9469=DIRECTION('ref_axis',(1.,0.,0.));
#9470=DIRECTION('center_axis',(0.,0.,1.));
#9471=DIRECTION('ref_axis',(-1.,-1.65389215948552E-15,0.));
#9472=DIRECTION('center_axis',(0.,0.,1.));
#9473=DIRECTION('ref_axis',(1.,0.,0.));
#9474=DIRECTION('center_axis',(0.,1.,0.));
#9475=DIRECTION('ref_axis',(1.,0.,0.));
#9476=DIRECTION('center_axis',(0.,1.,0.));
#9477=DIRECTION('ref_axis',(1.,0.,0.));
#9478=DIRECTION('',(0.,1.,0.));
#9479=DIRECTION('center_axis',(0.,-1.,0.));
#9480=DIRECTION('ref_axis',(1.,0.,0.));
#9481=DIRECTION('center_axis',(0.,1.,0.));
#9482=DIRECTION('ref_axis',(1.,0.,0.));
#9483=DIRECTION('center_axis',(0.,0.,1.));
#9484=DIRECTION('ref_axis',(1.,0.,0.));
#9485=DIRECTION('center_axis',(0.,0.,1.));
#9486=DIRECTION('ref_axis',(1.,0.,0.));
#9487=DIRECTION('center_axis',(0.,0.,1.));
#9488=DIRECTION('ref_axis',(1.,0.,0.));
#9489=DIRECTION('',(0.,0.,1.));
#9490=DIRECTION('center_axis',(0.,0.,-1.));
#9491=DIRECTION('ref_axis',(1.,0.,0.));
#9492=DIRECTION('center_axis',(0.,0.,1.));
#9493=DIRECTION('ref_axis',(1.,0.,0.));
#9494=DIRECTION('center_axis',(0.,1.,0.));
#9495=DIRECTION('ref_axis',(1.,0.,0.));
#9496=DIRECTION('center_axis',(0.,1.,0.));
#9497=DIRECTION('ref_axis',(1.,0.,0.));
#9498=DIRECTION('',(0.,1.,0.));
#9499=DIRECTION('center_axis',(0.,-1.,0.));
#9500=DIRECTION('ref_axis',(1.,0.,0.));
#9501=DIRECTION('center_axis',(0.,1.,0.));
#9502=DIRECTION('ref_axis',(1.,0.,0.));
#9503=DIRECTION('center_axis',(0.,1.,0.));
#9504=DIRECTION('ref_axis',(1.,0.,0.));
#9505=DIRECTION('',(0.,1.,0.));
#9506=DIRECTION('center_axis',(0.,-1.,0.));
#9507=DIRECTION('ref_axis',(1.,0.,0.));
#9508=DIRECTION('center_axis',(0.,1.,0.));
#9509=DIRECTION('ref_axis',(1.,0.,0.));
#9510=DIRECTION('center_axis',(0.,1.,0.));
#9511=DIRECTION('ref_axis',(1.,0.,0.));
#9512=DIRECTION('',(0.,1.,0.));
#9513=DIRECTION('center_axis',(0.,-1.,0.));
#9514=DIRECTION('ref_axis',(1.,0.,0.));
#9515=DIRECTION('center_axis',(0.,1.,0.));
#9516=DIRECTION('ref_axis',(1.,0.,0.));
#9517=DIRECTION('center_axis',(0.,1.,0.));
#9518=DIRECTION('ref_axis',(1.,0.,0.));
#9519=DIRECTION('',(0.,1.,0.));
#9520=DIRECTION('center_axis',(0.,-1.,0.));
#9521=DIRECTION('ref_axis',(1.,0.,0.));
#9522=DIRECTION('center_axis',(0.,1.,0.));
#9523=DIRECTION('ref_axis',(1.,0.,0.));
#9524=DIRECTION('center_axis',(0.,1.,0.));
#9525=DIRECTION('ref_axis',(1.,0.,0.));
#9526=DIRECTION('',(0.,1.,0.));
#9527=DIRECTION('center_axis',(0.,-1.,0.));
#9528=DIRECTION('ref_axis',(1.,0.,0.));
#9529=DIRECTION('center_axis',(0.,1.,0.));
#9530=DIRECTION('ref_axis',(1.,0.,0.));
#9531=DIRECTION('center_axis',(0.,1.,0.));
#9532=DIRECTION('ref_axis',(-1.,0.,0.));
#9533=DIRECTION('',(-1.,0.,0.));
#9534=DIRECTION('',(0.,0.,1.));
#9535=DIRECTION('',(-1.,0.,0.));
#9536=DIRECTION('',(0.,0.,1.));
#9537=DIRECTION('center_axis',(1.,0.,0.));
#9538=DIRECTION('ref_axis',(0.,1.,0.));
#9539=DIRECTION('',(0.,1.,0.));
#9540=DIRECTION('',(0.,1.,0.));
#9541=DIRECTION('',(0.,0.,1.));
#9542=DIRECTION('center_axis',(0.,-1.,0.));
#9543=DIRECTION('ref_axis',(1.,0.,0.));
#9544=DIRECTION('',(1.,0.,0.));
#9545=DIRECTION('',(1.,0.,0.));
#9546=DIRECTION('',(0.,0.,1.));
#9547=DIRECTION('center_axis',(-1.,0.,0.));
#9548=DIRECTION('ref_axis',(0.,-1.,0.));
#9549=DIRECTION('',(0.,-1.,0.));
#9550=DIRECTION('',(0.,-1.,0.));
#9551=DIRECTION('center_axis',(0.,0.,1.));
#9552=DIRECTION('ref_axis',(1.,0.,0.));
#9553=DIRECTION('center_axis',(0.,0.,1.));
#9554=DIRECTION('ref_axis',(1.,0.,0.));
#9555=DIRECTION('axis',(0.,0.,1.));
#9556=DIRECTION('refdir',(1.,0.,0.));
#9557=DIRECTION('center_axis',(1.,0.,0.));
#9558=DIRECTION('ref_axis',(0.,0.,-1.));
#9559=DIRECTION('center_axis',(1.,0.,0.));
#9560=DIRECTION('ref_axis',(0.,0.,-1.));
#9561=DIRECTION('',(1.,0.,0.));
#9562=DIRECTION('center_axis',(-1.,0.,0.));
#9563=DIRECTION('ref_axis',(0.,0.,-1.));
#9564=DIRECTION('center_axis',(1.,0.,0.));
#9565=DIRECTION('ref_axis',(0.,0.,-1.));
#9566=DIRECTION('',(0.,0.,-1.));
#9567=DIRECTION('',(0.,-1.,0.));
#9568=DIRECTION('',(0.,0.,1.));
#9569=DIRECTION('',(0.,1.,0.));
#9570=DIRECTION('center_axis',(0.,0.,1.));
#9571=DIRECTION('ref_axis',(1.,0.,0.));
#9572=DIRECTION('center_axis',(0.,0.,1.));
#9573=DIRECTION('ref_axis',(1.,0.,0.));
#9574=DIRECTION('center_axis',(0.,0.,1.));
#9575=DIRECTION('ref_axis',(1.,0.,0.));
#9576=DIRECTION('center_axis',(0.,0.,1.));
#9577=DIRECTION('ref_axis',(-1.,1.22464679914735E-16,0.));
#9578=DIRECTION('center_axis',(0.,0.,1.));
#9579=DIRECTION('ref_axis',(1.,0.,0.));
#9580=DIRECTION('center_axis',(0.,0.,1.));
#9581=DIRECTION('ref_axis',(1.,0.,0.));
#9582=DIRECTION('center_axis',(0.,0.,1.));
#9583=DIRECTION('ref_axis',(1.,0.,0.));
#9584=DIRECTION('',(0.,0.,1.));
#9585=DIRECTION('center_axis',(0.,0.,1.));
#9586=DIRECTION('ref_axis',(1.,0.,0.));
#9587=DIRECTION('center_axis',(0.,0.,1.));
#9588=DIRECTION('ref_axis',(1.,0.,0.));
#9589=DIRECTION('center_axis',(0.,0.,-1.));
#9590=DIRECTION('ref_axis',(1.,0.,0.));
#9591=DIRECTION('center_axis',(0.,0.,1.));
#9592=DIRECTION('ref_axis',(1.,0.,0.));
#9593=DIRECTION('center_axis',(0.,0.,1.));
#9594=DIRECTION('ref_axis',(1.,0.,0.));
#9595=DIRECTION('center_axis',(0.,0.,1.));
#9596=DIRECTION('ref_axis',(1.,0.,0.));
#9597=DIRECTION('',(0.,0.,1.));
#9598=DIRECTION('center_axis',(0.,0.,1.));
#9599=DIRECTION('ref_axis',(1.,0.,0.));
#9600=DIRECTION('',(0.,0.,1.));
#9601=DIRECTION('center_axis',(0.,0.,-1.));
#9602=DIRECTION('ref_axis',(1.,0.,0.));
#9603=DIRECTION('center_axis',(0.,0.,1.));
#9604=DIRECTION('ref_axis',(1.,0.,0.));
#9605=DIRECTION('center_axis',(0.,0.,1.));
#9606=DIRECTION('ref_axis',(1.,0.,0.));
#9607=DIRECTION('center_axis',(0.,0.,1.));
#9608=DIRECTION('ref_axis',(1.,0.,0.));
#9609=DIRECTION('',(0.5,-0.866025403784439,0.));
#9610=DIRECTION('',(1.,-3.43386193997065E-16,0.));
#9611=DIRECTION('',(0.5,0.866025403784439,0.));
#9612=DIRECTION('',(0.,1.,0.));
#9613=DIRECTION('',(1.,0.,0.));
#9614=DIRECTION('',(0.,-1.,0.));
#9615=DIRECTION('center_axis',(0.,1.,0.));
#9616=DIRECTION('ref_axis',(-1.,0.,0.));
#9617=DIRECTION('',(-1.,0.,0.));
#9618=DIRECTION('',(0.,0.,1.));
#9619=DIRECTION('',(-1.,0.,0.));
#9620=DIRECTION('',(0.,0.,1.));
#9621=DIRECTION('center_axis',(1.,0.,0.));
#9622=DIRECTION('ref_axis',(0.,1.,0.));
#9623=DIRECTION('',(0.,-1.,0.));
#9624=DIRECTION('',(0.,1.,0.));
#9625=DIRECTION('',(0.,1.,0.));
#9626=DIRECTION('',(0.,0.,1.));
#9627=DIRECTION('center_axis',(0.,-1.,0.));
#9628=DIRECTION('ref_axis',(1.,0.,0.));
#9629=DIRECTION('',(1.,0.,0.));
#9630=DIRECTION('',(0.,0.,1.));
#9631=DIRECTION('center_axis',(-1.,0.,0.));
#9632=DIRECTION('ref_axis',(0.,-1.,0.));
#9633=DIRECTION('',(0.,-1.,0.));
#9634=DIRECTION('',(0.,1.,0.));
#9635=DIRECTION('',(0.,-1.,0.));
#9636=DIRECTION('center_axis',(0.,0.,1.));
#9637=DIRECTION('ref_axis',(1.,0.,0.));
#9638=DIRECTION('center_axis',(0.,0.,1.));
#9639=DIRECTION('ref_axis',(1.,0.,0.));
#9640=DIRECTION('',(-0.5,-0.866025403784439,0.));
#9641=DIRECTION('',(-0.5,0.866025403784439,0.));
#9642=DIRECTION('',(-1.,0.,0.));
#9643=DIRECTION('center_axis',(0.,0.,1.));
#9644=DIRECTION('ref_axis',(1.,0.,0.));
#9645=DIRECTION('',(0.5,0.866025403784439,0.));
#9646=DIRECTION('',(-0.5,0.866025403784439,0.));
#9647=DIRECTION('center_axis',(0.,0.,1.));
#9648=DIRECTION('ref_axis',(1.,0.,0.));
#9649=DIRECTION('',(0.5,0.866025403784439,0.));
#9650=DIRECTION('',(1.,-3.43386193997065E-16,0.));
#9651=DIRECTION('',(0.5,-0.866025403784439,0.));
#9652=DIRECTION('',(-0.5,-0.866025403784438,0.));
#9653=DIRECTION('',(-1.,0.,0.));
#9654=DIRECTION('',(-0.5,0.866025403784439,0.));
#9655=DIRECTION('center_axis',(0.,0.,1.));
#9656=DIRECTION('ref_axis',(1.,0.,0.));
#9657=DIRECTION('center_axis',(-3.43386193997065E-16,-1.,0.));
#9658=DIRECTION('ref_axis',(1.,-3.43386193997065E-16,0.));
#9659=DIRECTION('',(0.,0.,1.));
#9660=DIRECTION('',(0.,0.,1.));
#9661=DIRECTION('center_axis',(-0.866025403784439,-0.5,0.));
#9662=DIRECTION('ref_axis',(0.5,-0.866025403784439,0.));
#9663=DIRECTION('',(0.5,-0.866025403784439,0.));
#9664=DIRECTION('',(0.,0.,1.));
#9665=DIRECTION('center_axis',(-0.866025403784439,0.5,0.));
#9666=DIRECTION('ref_axis',(-0.5,-0.866025403784439,0.));
#9667=DIRECTION('',(-0.5,-0.866025403784438,0.));
#9668=DIRECTION('',(0.,0.,1.));
#9669=DIRECTION('center_axis',(0.,1.,0.));
#9670=DIRECTION('ref_axis',(-1.,0.,0.));
#9671=DIRECTION('',(0.,0.,1.));
#9672=DIRECTION('center_axis',(0.866025403784439,0.5,0.));
#9673=DIRECTION('ref_axis',(-0.5,0.866025403784439,0.));
#9674=DIRECTION('',(0.,0.,1.));
#9675=DIRECTION('center_axis',(0.866025403784439,-0.5,0.));
#9676=DIRECTION('ref_axis',(0.5,0.866025403784439,0.));
#9677=DIRECTION('center_axis',(0.,0.,1.));
#9678=DIRECTION('ref_axis',(1.,0.,0.));
#9679=DIRECTION('center_axis',(0.,0.,1.));
#9680=DIRECTION('ref_axis',(1.,0.,0.));
#9681=DIRECTION('',(0.,0.,-1.));
#9682=DIRECTION('center_axis',(0.,0.,-1.));
#9683=DIRECTION('ref_axis',(1.,0.,0.));
#9684=DIRECTION('center_axis',(0.,0.,1.));
#9685=DIRECTION('ref_axis',(1.,0.,0.));
#9686=DIRECTION('',(0.,0.,-1.));
#9687=DIRECTION('center_axis',(0.,0.,1.));
#9688=DIRECTION('ref_axis',(1.,0.,0.));
#9689=DIRECTION('center_axis',(0.,0.,1.));
#9690=DIRECTION('ref_axis',(1.,0.,0.));
#9691=DIRECTION('axis',(0.,0.,1.));
#9692=DIRECTION('refdir',(1.,0.,0.));
#9693=DIRECTION('center_axis',(0.,0.,1.));
#9694=DIRECTION('ref_axis',(1.,0.,0.));
#9695=DIRECTION('center_axis',(0.,0.,1.));
#9696=DIRECTION('ref_axis',(1.,0.,0.));
#9697=DIRECTION('',(0.707106781186549,8.65956056235495E-17,-0.707106781186546));
#9698=DIRECTION('center_axis',(0.,0.,1.));
#9699=DIRECTION('ref_axis',(1.,0.,0.));
#9700=DIRECTION('center_axis',(0.,0.,1.));
#9701=DIRECTION('ref_axis',(1.,0.,0.));
#9702=DIRECTION('',(0.316227766016837,3.87267321454038E-17,-0.948683298050514));
#9703=DIRECTION('center_axis',(0.,0.,1.));
#9704=DIRECTION('ref_axis',(1.,0.,0.));
#9705=DIRECTION('center_axis',(0.,0.,1.));
#9706=DIRECTION('ref_axis',(1.,0.,0.));
#9707=DIRECTION('',(0.,0.,-1.));
#9708=DIRECTION('center_axis',(0.,0.,-1.));
#9709=DIRECTION('ref_axis',(-1.,0.,0.));
#9710=DIRECTION('center_axis',(0.,0.,1.));
#9711=DIRECTION('ref_axis',(1.,0.,0.));
#9712=DIRECTION('center_axis',(0.,0.,1.));
#9713=DIRECTION('ref_axis',(1.,0.,0.));
#9714=DIRECTION('center_axis',(0.,0.,1.));
#9715=DIRECTION('ref_axis',(1.,0.,0.));
#9716=DIRECTION('',(0.,0.,-1.));
#9717=DIRECTION('center_axis',(0.,0.,1.));
#9718=DIRECTION('ref_axis',(1.,0.,0.));
#9719=DIRECTION('axis',(0.,0.,1.));
#9720=DIRECTION('refdir',(1.,0.,0.));
#9721=DIRECTION('center_axis',(0.,0.,1.));
#9722=DIRECTION('ref_axis',(1.,0.,0.));
#9723=DIRECTION('center_axis',(0.,0.,1.));
#9724=DIRECTION('ref_axis',(1.,0.,0.));
#9725=DIRECTION('',(0.,0.,1.));
#9726=DIRECTION('center_axis',(0.,0.,1.));
#9727=DIRECTION('ref_axis',(1.,0.,0.));
#9728=DIRECTION('center_axis',(0.,0.,1.));
#9729=DIRECTION('ref_axis',(1.,0.,0.));
#9730=DIRECTION('center_axis',(0.,0.,1.));
#9731=DIRECTION('ref_axis',(1.,0.,0.));
#9732=DIRECTION('center_axis',(0.,0.,1.));
#9733=DIRECTION('ref_axis',(1.,0.,0.));
#9734=DIRECTION('',(0.,0.,1.));
#9735=DIRECTION('center_axis',(0.,0.,1.));
#9736=DIRECTION('ref_axis',(1.,0.,0.));
#9737=DIRECTION('center_axis',(0.,0.,1.));
#9738=DIRECTION('ref_axis',(1.,0.,0.));
#9739=DIRECTION('center_axis',(0.,1.,0.));
#9740=DIRECTION('ref_axis',(1.,0.,0.));
#9741=DIRECTION('',(1.,0.,0.));
#9742=DIRECTION('center_axis',(0.,1.,0.));
#9743=DIRECTION('ref_axis',(1.,0.,0.));
#9744=DIRECTION('center_axis',(0.,1.,0.));
#9745=DIRECTION('ref_axis',(1.,0.,0.));
#9746=DIRECTION('',(0.,0.,1.));
#9747=DIRECTION('center_axis',(0.,1.,0.));
#9748=DIRECTION('ref_axis',(1.,0.,0.));
#9749=DIRECTION('center_axis',(0.,1.,0.));
#9750=DIRECTION('ref_axis',(1.,0.,0.));
#9751=DIRECTION('',(0.,0.,-1.));
#9752=DIRECTION('center_axis',(0.,1.,0.));
#9753=DIRECTION('ref_axis',(1.,0.,0.));
#9754=DIRECTION('center_axis',(0.,1.,0.));
#9755=DIRECTION('ref_axis',(1.,0.,0.));
#9756=DIRECTION('',(0.,1.,0.));
#9757=DIRECTION('center_axis',(0.,1.,0.));
#9758=DIRECTION('ref_axis',(1.,0.,0.));
#9759=DIRECTION('',(0.,-1.,0.));
#9760=DIRECTION('center_axis',(0.,1.,0.));
#9761=DIRECTION('ref_axis',(1.,0.,0.));
#9762=DIRECTION('',(0.,1.,0.));
#9763=DIRECTION('center_axis',(0.,-0.707106781186549,-0.707106781186546));
#9764=DIRECTION('ref_axis',(0.,0.707106781186546,-0.707106781186549));
#9765=DIRECTION('center_axis',(0.,-0.707106781186549,0.707106781186546));
#9766=DIRECTION('ref_axis',(0.,-0.707106781186546,-0.707106781186549));
#9767=DIRECTION('',(0.,-1.,0.));
#9768=DIRECTION('',(0.,1.,0.));
#9769=DIRECTION('center_axis',(0.,-0.707106781186549,0.707106781186546));
#9770=DIRECTION('ref_axis',(0.,-0.707106781186546,-0.707106781186549));
#9771=DIRECTION('center_axis',(0.,1.,0.));
#9772=DIRECTION('ref_axis',(1.,0.,0.));
#9773=DIRECTION('center_axis',(0.,1.,0.));
#9774=DIRECTION('ref_axis',(1.,0.,0.));
#9775=DIRECTION('center_axis',(0.,0.707106781186549,-0.707106781186546));
#9776=DIRECTION('ref_axis',(0.,-0.707106781186546,-0.707106781186549));
#9777=DIRECTION('center_axis',(0.,0.707106781186549,0.707106781186546));
#9778=DIRECTION('ref_axis',(0.,0.707106781186546,-0.707106781186549));
#9779=DIRECTION('center_axis',(0.,1.,0.));
#9780=DIRECTION('ref_axis',(-1.,0.,1.22464679914735E-16));
#9781=DIRECTION('center_axis',(0.,0.707106781186549,-0.707106781186546));
#9782=DIRECTION('ref_axis',(0.,-0.707106781186546,-0.707106781186549));
#9783=DIRECTION('center_axis',(0.,0.707106781186549,0.707106781186546));
#9784=DIRECTION('ref_axis',(0.,0.707106781186546,-0.707106781186549));
#9785=DIRECTION('center_axis',(0.,1.,0.));
#9786=DIRECTION('ref_axis',(1.,0.,0.));
#9787=DIRECTION('center_axis',(0.,1.,0.));
#9788=DIRECTION('ref_axis',(1.,0.,0.));
#9789=DIRECTION('center_axis',(0.,0.,1.));
#9790=DIRECTION('ref_axis',(1.,0.,0.));
#9791=DIRECTION('center_axis',(0.,0.,1.));
#9792=DIRECTION('ref_axis',(1.,0.,0.));
#9793=DIRECTION('center_axis',(0.,0.,1.));
#9794=DIRECTION('ref_axis',(1.,0.,0.));
#9795=DIRECTION('center_axis',(0.,0.,1.));
#9796=DIRECTION('ref_axis',(1.,0.,0.));
#9797=DIRECTION('center_axis',(0.,0.,1.));
#9798=DIRECTION('ref_axis',(1.,0.,0.));
#9799=DIRECTION('center_axis',(0.,0.,1.));
#9800=DIRECTION('ref_axis',(1.,0.,0.));
#9801=DIRECTION('center_axis',(0.,0.,1.));
#9802=DIRECTION('ref_axis',(1.,0.,0.));
#9803=DIRECTION('center_axis',(0.,0.,1.));
#9804=DIRECTION('ref_axis',(-1.,5.20660583828602E-15,0.));
#9805=DIRECTION('center_axis',(0.,0.,1.));
#9806=DIRECTION('ref_axis',(1.,0.,0.));
#9807=DIRECTION('',(0.,0.,1.));
#9808=DIRECTION('center_axis',(0.,0.,-1.));
#9809=DIRECTION('ref_axis',(1.,0.,0.));
#9810=DIRECTION('center_axis',(0.,1.,0.));
#9811=DIRECTION('ref_axis',(1.,0.,0.));
#9812=DIRECTION('center_axis',(0.,1.,0.));
#9813=DIRECTION('ref_axis',(1.,0.,0.));
#9814=DIRECTION('center_axis',(0.,1.,0.));
#9815=DIRECTION('ref_axis',(1.,0.,0.));
#9816=DIRECTION('center_axis',(0.,0.,1.));
#9817=DIRECTION('ref_axis',(1.,0.,0.));
#9818=DIRECTION('center_axis',(0.,0.,1.));
#9819=DIRECTION('ref_axis',(1.,0.,0.));
#9820=DIRECTION('',(0.,0.,1.));
#9821=DIRECTION('center_axis',(0.,0.,-1.));
#9822=DIRECTION('ref_axis',(1.,0.,0.));
#9823=DIRECTION('center_axis',(0.,0.,1.));
#9824=DIRECTION('ref_axis',(1.,0.,0.));
#9825=DIRECTION('center_axis',(0.,1.,0.));
#9826=DIRECTION('ref_axis',(1.,0.,0.));
#9827=DIRECTION('center_axis',(0.,1.,0.));
#9828=DIRECTION('ref_axis',(1.,0.,0.));
#9829=DIRECTION('',(0.,1.,0.));
#9830=DIRECTION('center_axis',(0.,-1.,0.));
#9831=DIRECTION('ref_axis',(1.,0.,0.));
#9832=DIRECTION('center_axis',(0.,1.,0.));
#9833=DIRECTION('ref_axis',(1.,0.,0.));
#9834=DIRECTION('center_axis',(0.,1.,0.));
#9835=DIRECTION('ref_axis',(1.,0.,0.));
#9836=DIRECTION('',(0.,1.,0.));
#9837=DIRECTION('center_axis',(0.,-1.,0.));
#9838=DIRECTION('ref_axis',(1.,0.,0.));
#9839=DIRECTION('center_axis',(0.,1.,0.));
#9840=DIRECTION('ref_axis',(1.,0.,0.));
#9841=DIRECTION('center_axis',(0.,1.,0.));
#9842=DIRECTION('ref_axis',(1.,0.,0.));
#9843=DIRECTION('',(0.,1.,0.));
#9844=DIRECTION('center_axis',(0.,-1.,0.));
#9845=DIRECTION('ref_axis',(1.,0.,0.));
#9846=DIRECTION('center_axis',(0.,1.,0.));
#9847=DIRECTION('ref_axis',(1.,0.,0.));
#9848=DIRECTION('center_axis',(0.,1.,0.));
#9849=DIRECTION('ref_axis',(1.,0.,0.));
#9850=DIRECTION('',(0.,1.,0.));
#9851=DIRECTION('center_axis',(0.,-1.,0.));
#9852=DIRECTION('ref_axis',(1.,0.,0.));
#9853=DIRECTION('center_axis',(0.,1.,0.));
#9854=DIRECTION('ref_axis',(1.,0.,0.));
#9855=DIRECTION('center_axis',(0.,1.,0.));
#9856=DIRECTION('ref_axis',(1.,0.,0.));
#9857=DIRECTION('',(0.,1.,0.));
#9858=DIRECTION('center_axis',(0.,1.,0.));
#9859=DIRECTION('ref_axis',(-1.,0.,0.));
#9860=DIRECTION('',(-1.,0.,0.));
#9861=DIRECTION('',(0.,0.,1.));
#9862=DIRECTION('',(-1.,0.,0.));
#9863=DIRECTION('',(0.,0.,1.));
#9864=DIRECTION('center_axis',(1.,0.,0.));
#9865=DIRECTION('ref_axis',(0.,1.,0.));
#9866=DIRECTION('',(0.,1.,0.));
#9867=DIRECTION('',(0.,1.,0.));
#9868=DIRECTION('',(0.,0.,1.));
#9869=DIRECTION('center_axis',(0.,-1.,0.));
#9870=DIRECTION('ref_axis',(1.,0.,0.));
#9871=DIRECTION('',(1.,0.,0.));
#9872=DIRECTION('',(1.,0.,0.));
#9873=DIRECTION('',(0.,0.,1.));
#9874=DIRECTION('center_axis',(-1.,0.,0.));
#9875=DIRECTION('ref_axis',(0.,-1.,0.));
#9876=DIRECTION('',(0.,-1.,0.));
#9877=DIRECTION('',(0.,-1.,0.));
#9878=DIRECTION('center_axis',(0.,0.,1.));
#9879=DIRECTION('ref_axis',(1.,0.,0.));
#9880=DIRECTION('center_axis',(0.,0.,1.));
#9881=DIRECTION('ref_axis',(1.,0.,0.));
#9882=DIRECTION('axis',(0.,0.,1.));
#9883=DIRECTION('refdir',(1.,0.,0.));
#9884=DIRECTION('center_axis',(1.,0.,0.));
#9885=DIRECTION('ref_axis',(0.,0.,-1.));
#9886=DIRECTION('center_axis',(1.,0.,0.));
#9887=DIRECTION('ref_axis',(0.,0.,-1.));
#9888=DIRECTION('',(1.,0.,0.));
#9889=DIRECTION('center_axis',(-1.,0.,0.));
#9890=DIRECTION('ref_axis',(0.,0.,-1.));
#9891=DIRECTION('center_axis',(1.,0.,0.));
#9892=DIRECTION('ref_axis',(0.,0.,-1.));
#9893=DIRECTION('',(0.,0.,-1.));
#9894=DIRECTION('',(0.,-1.,0.));
#9895=DIRECTION('',(0.,0.,1.));
#9896=DIRECTION('',(0.,1.,0.));
#9897=DIRECTION('center_axis',(0.,0.,1.));
#9898=DIRECTION('ref_axis',(1.,0.,0.));
#9899=DIRECTION('center_axis',(0.,0.,1.));
#9900=DIRECTION('ref_axis',(1.,0.,0.));
#9901=DIRECTION('center_axis',(0.,0.,1.));
#9902=DIRECTION('ref_axis',(1.,0.,0.));
#9903=DIRECTION('center_axis',(0.,0.,1.));
#9904=DIRECTION('ref_axis',(-1.,1.22464679914735E-16,0.));
#9905=DIRECTION('center_axis',(0.,0.,1.));
#9906=DIRECTION('ref_axis',(1.,0.,0.));
#9907=DIRECTION('center_axis',(0.,0.,1.));
#9908=DIRECTION('ref_axis',(1.,0.,0.));
#9909=DIRECTION('center_axis',(0.,0.,1.));
#9910=DIRECTION('ref_axis',(1.,0.,0.));
#9911=DIRECTION('',(0.,0.,1.));
#9912=DIRECTION('center_axis',(0.,0.,1.));
#9913=DIRECTION('ref_axis',(1.,0.,0.));
#9914=DIRECTION('center_axis',(0.,0.,1.));
#9915=DIRECTION('ref_axis',(1.,0.,0.));
#9916=DIRECTION('center_axis',(0.,0.,-1.));
#9917=DIRECTION('ref_axis',(1.,0.,0.));
#9918=DIRECTION('center_axis',(0.,0.,1.));
#9919=DIRECTION('ref_axis',(1.,0.,0.));
#9920=DIRECTION('center_axis',(0.,0.,1.));
#9921=DIRECTION('ref_axis',(1.,0.,0.));
#9922=DIRECTION('center_axis',(0.,0.,1.));
#9923=DIRECTION('ref_axis',(1.,0.,0.));
#9924=DIRECTION('',(0.,0.,1.));
#9925=DIRECTION('center_axis',(0.,0.,1.));
#9926=DIRECTION('ref_axis',(1.,0.,0.));
#9927=DIRECTION('',(0.,0.,1.));
#9928=DIRECTION('center_axis',(0.,0.,-1.));
#9929=DIRECTION('ref_axis',(1.,0.,0.));
#9930=DIRECTION('center_axis',(0.,0.,1.));
#9931=DIRECTION('ref_axis',(1.,0.,0.));
#9932=DIRECTION('center_axis',(0.,0.,1.));
#9933=DIRECTION('ref_axis',(1.,0.,0.));
#9934=DIRECTION('center_axis',(0.,0.,1.));
#9935=DIRECTION('ref_axis',(1.,0.,0.));
#9936=DIRECTION('',(0.5,-0.866025403784439,0.));
#9937=DIRECTION('',(1.,0.,0.));
#9938=DIRECTION('',(0.5,0.866025403784439,0.));
#9939=DIRECTION('',(0.,1.,0.));
#9940=DIRECTION('',(1.,0.,0.));
#9941=DIRECTION('',(0.,-1.,0.));
#9942=DIRECTION('center_axis',(0.,1.,0.));
#9943=DIRECTION('ref_axis',(-1.,0.,0.));
#9944=DIRECTION('',(-1.,0.,0.));
#9945=DIRECTION('',(0.,0.,1.));
#9946=DIRECTION('',(-1.,0.,0.));
#9947=DIRECTION('',(0.,0.,1.));
#9948=DIRECTION('center_axis',(1.,0.,0.));
#9949=DIRECTION('ref_axis',(0.,1.,0.));
#9950=DIRECTION('',(0.,-1.,0.));
#9951=DIRECTION('',(0.,1.,0.));
#9952=DIRECTION('',(0.,1.,0.));
#9953=DIRECTION('',(0.,0.,1.));
#9954=DIRECTION('center_axis',(0.,-1.,0.));
#9955=DIRECTION('ref_axis',(1.,0.,0.));
#9956=DIRECTION('',(1.,0.,0.));
#9957=DIRECTION('',(0.,0.,1.));
#9958=DIRECTION('center_axis',(-1.,0.,0.));
#9959=DIRECTION('ref_axis',(0.,-1.,0.));
#9960=DIRECTION('',(0.,-1.,0.));
#9961=DIRECTION('',(0.,1.,0.));
#9962=DIRECTION('',(0.,-1.,0.));
#9963=DIRECTION('center_axis',(0.,0.,1.));
#9964=DIRECTION('ref_axis',(1.,0.,0.));
#9965=DIRECTION('center_axis',(0.,0.,1.));
#9966=DIRECTION('ref_axis',(1.,0.,0.));
#9967=DIRECTION('',(-0.5,-0.866025403784439,0.));
#9968=DIRECTION('',(-0.5,0.866025403784439,0.));
#9969=DIRECTION('',(-1.,0.,0.));
#9970=DIRECTION('center_axis',(0.,0.,1.));
#9971=DIRECTION('ref_axis',(1.,0.,0.));
#9972=DIRECTION('',(0.5,0.866025403784439,0.));
#9973=DIRECTION('',(-0.5,0.866025403784439,0.));
#9974=DIRECTION('center_axis',(0.,0.,1.));
#9975=DIRECTION('ref_axis',(1.,0.,0.));
#9976=DIRECTION('',(0.5,0.866025403784439,0.));
#9977=DIRECTION('',(1.,0.,0.));
#9978=DIRECTION('',(0.5,-0.866025403784439,0.));
#9979=DIRECTION('',(-0.5,-0.866025403784439,0.));
#9980=DIRECTION('',(-1.,0.,0.));
#9981=DIRECTION('',(-0.5,0.866025403784439,0.));
#9982=DIRECTION('center_axis',(0.,0.,1.));
#9983=DIRECTION('ref_axis',(1.,0.,0.));
#9984=DIRECTION('center_axis',(0.,-1.,0.));
#9985=DIRECTION('ref_axis',(1.,0.,0.));
#9986=DIRECTION('',(0.,0.,1.));
#9987=DIRECTION('',(0.,0.,1.));
#9988=DIRECTION('center_axis',(-0.866025403784439,-0.5,0.));
#9989=DIRECTION('ref_axis',(0.5,-0.866025403784439,0.));
#9990=DIRECTION('',(0.5,-0.866025403784439,0.));
#9991=DIRECTION('',(0.,0.,1.));
#9992=DIRECTION('center_axis',(-0.866025403784439,0.5,0.));
#9993=DIRECTION('ref_axis',(-0.5,-0.866025403784439,0.));
#9994=DIRECTION('',(-0.5,-0.866025403784439,0.));
#9995=DIRECTION('',(0.,0.,1.));
#9996=DIRECTION('center_axis',(0.,1.,0.));
#9997=DIRECTION('ref_axis',(-1.,0.,0.));
#9998=DIRECTION('',(0.,0.,1.));
#9999=DIRECTION('center_axis',(0.866025403784439,0.5,0.));
#10000=DIRECTION('ref_axis',(-0.5,0.866025403784439,0.));
#10001=DIRECTION('',(0.,0.,1.));
#10002=DIRECTION('center_axis',(0.866025403784439,-0.5,0.));
#10003=DIRECTION('ref_axis',(0.5,0.866025403784439,0.));
#10004=DIRECTION('center_axis',(0.,0.,1.));
#10005=DIRECTION('ref_axis',(1.,0.,0.));
#10006=DIRECTION('center_axis',(0.,0.,1.));
#10007=DIRECTION('ref_axis',(1.,0.,0.));
#10008=DIRECTION('',(0.,0.,-1.));
#10009=DIRECTION('center_axis',(0.,0.,-1.));
#10010=DIRECTION('ref_axis',(1.,0.,0.));
#10011=DIRECTION('center_axis',(0.,0.,1.));
#10012=DIRECTION('ref_axis',(1.,0.,0.));
#10013=DIRECTION('',(0.,0.,-1.));
#10014=DIRECTION('center_axis',(0.,0.,1.));
#10015=DIRECTION('ref_axis',(1.,0.,0.));
#10016=DIRECTION('center_axis',(0.,0.,1.));
#10017=DIRECTION('ref_axis',(1.,0.,0.));
#10018=DIRECTION('axis',(0.,0.,1.));
#10019=DIRECTION('refdir',(1.,0.,0.));
#10020=DIRECTION('center_axis',(0.,0.,1.));
#10021=DIRECTION('ref_axis',(1.,0.,0.));
#10022=DIRECTION('center_axis',(0.,0.,1.));
#10023=DIRECTION('ref_axis',(1.,0.,0.));
#10024=DIRECTION('',(0.707106781186549,8.65956056235495E-17,-0.707106781186546));
#10025=DIRECTION('center_axis',(0.,0.,1.));
#10026=DIRECTION('ref_axis',(1.,0.,0.));
#10027=DIRECTION('center_axis',(0.,0.,1.));
#10028=DIRECTION('ref_axis',(1.,0.,0.));
#10029=DIRECTION('',(0.316227766016837,3.87267321454038E-17,-0.948683298050514));
#10030=DIRECTION('center_axis',(0.,0.,1.));
#10031=DIRECTION('ref_axis',(1.,0.,0.));
#10032=DIRECTION('center_axis',(0.,0.,1.));
#10033=DIRECTION('ref_axis',(1.,0.,0.));
#10034=DIRECTION('',(0.,0.,-1.));
#10035=DIRECTION('center_axis',(0.,0.,-1.));
#10036=DIRECTION('ref_axis',(-1.,0.,0.));
#10037=DIRECTION('center_axis',(0.,0.,1.));
#10038=DIRECTION('ref_axis',(1.,0.,0.));
#10039=DIRECTION('center_axis',(0.,0.,1.));
#10040=DIRECTION('ref_axis',(1.,0.,0.));
#10041=DIRECTION('center_axis',(0.,0.,1.));
#10042=DIRECTION('ref_axis',(1.,0.,0.));
#10043=DIRECTION('',(0.,0.,-1.));
#10044=DIRECTION('center_axis',(0.,0.,1.));
#10045=DIRECTION('ref_axis',(1.,0.,0.));
#10046=DIRECTION('axis',(0.,0.,1.));
#10047=DIRECTION('refdir',(1.,0.,0.));
#10048=DIRECTION('center_axis',(0.,1.,0.));
#10049=DIRECTION('ref_axis',(1.,0.,0.));
#10050=DIRECTION('center_axis',(0.,-1.,0.));
#10051=DIRECTION('ref_axis',(1.,0.,0.));
#10052=DIRECTION('',(0.,-1.,0.));
#10053=DIRECTION('center_axis',(0.,-1.,0.));
#10054=DIRECTION('ref_axis',(1.,0.,0.));
#10055=DIRECTION('center_axis',(0.,1.,0.));
#10056=DIRECTION('ref_axis',(1.,0.,0.));
#10057=DIRECTION('center_axis',(0.,1.,0.));
#10058=DIRECTION('ref_axis',(1.,0.,0.));
#10059=DIRECTION('',(0.,-1.,0.));
#10060=DIRECTION('center_axis',(0.,1.,0.));
#10061=DIRECTION('ref_axis',(1.,0.,0.));
#10062=DIRECTION('center_axis',(0.,1.,0.));
#10063=DIRECTION('ref_axis',(1.,0.,0.));
#10064=DIRECTION('center_axis',(0.,1.,0.));
#10065=DIRECTION('ref_axis',(1.,0.,0.));
#10066=DIRECTION('axis',(0.,0.,1.));
#10067=DIRECTION('refdir',(1.,0.,0.));
#10068=DIRECTION('center_axis',(0.,1.,0.));
#10069=DIRECTION('ref_axis',(1.,0.,0.));
#10070=DIRECTION('center_axis',(0.,-1.,0.));
#10071=DIRECTION('ref_axis',(1.,0.,0.));
#10072=DIRECTION('',(0.,-1.,0.));
#10073=DIRECTION('center_axis',(0.,-1.,0.));
#10074=DIRECTION('ref_axis',(1.,0.,0.));
#10075=DIRECTION('center_axis',(0.,1.,0.));
#10076=DIRECTION('ref_axis',(1.,0.,0.));
#10077=DIRECTION('center_axis',(0.,1.,0.));
#10078=DIRECTION('ref_axis',(1.,0.,0.));
#10079=DIRECTION('',(0.,-1.,0.));
#10080=DIRECTION('center_axis',(0.,1.,0.));
#10081=DIRECTION('ref_axis',(1.,0.,0.));
#10082=DIRECTION('center_axis',(0.,1.,0.));
#10083=DIRECTION('ref_axis',(1.,0.,0.));
#10084=DIRECTION('center_axis',(0.,1.,0.));
#10085=DIRECTION('ref_axis',(1.,0.,0.));
#10086=DIRECTION('axis',(0.,0.,1.));
#10087=DIRECTION('refdir',(1.,0.,0.));
#10088=DIRECTION('center_axis',(0.,1.,0.));
#10089=DIRECTION('ref_axis',(1.,0.,0.));
#10090=DIRECTION('center_axis',(0.,-1.,0.));
#10091=DIRECTION('ref_axis',(1.,0.,0.));
#10092=DIRECTION('',(0.,-1.,0.));
#10093=DIRECTION('center_axis',(0.,-1.,0.));
#10094=DIRECTION('ref_axis',(1.,0.,0.));
#10095=DIRECTION('center_axis',(0.,1.,0.));
#10096=DIRECTION('ref_axis',(1.,0.,0.));
#10097=DIRECTION('center_axis',(0.,1.,0.));
#10098=DIRECTION('ref_axis',(1.,0.,0.));
#10099=DIRECTION('',(0.,-1.,0.));
#10100=DIRECTION('center_axis',(0.,1.,0.));
#10101=DIRECTION('ref_axis',(1.,0.,0.));
#10102=DIRECTION('center_axis',(0.,1.,0.));
#10103=DIRECTION('ref_axis',(1.,0.,0.));
#10104=DIRECTION('center_axis',(0.,1.,0.));
#10105=DIRECTION('ref_axis',(1.,0.,0.));
#10106=DIRECTION('axis',(0.,0.,1.));
#10107=DIRECTION('refdir',(1.,0.,0.));
#10108=DIRECTION('center_axis',(0.,0.,1.));
#10109=DIRECTION('ref_axis',(1.,0.,0.));
#10110=DIRECTION('center_axis',(0.,0.,1.));
#10111=DIRECTION('ref_axis',(1.,0.,0.));
#10112=DIRECTION('',(0.,0.,1.));
#10113=DIRECTION('center_axis',(0.,0.,-1.));
#10114=DIRECTION('ref_axis',(1.,0.,0.));
#10115=DIRECTION('center_axis',(0.,0.,1.));
#10116=DIRECTION('ref_axis',(1.,0.,0.));
#10117=DIRECTION('center_axis',(0.,0.,1.));
#10118=DIRECTION('ref_axis',(1.,0.,0.));
#10119=DIRECTION('center_axis',(0.,0.,1.));
#10120=DIRECTION('ref_axis',(1.,0.,0.));
#10121=DIRECTION('center_axis',(0.,0.,1.));
#10122=DIRECTION('ref_axis',(1.,0.,0.));
#10123=DIRECTION('',(0.,0.,1.));
#10124=DIRECTION('center_axis',(0.,0.,-1.));
#10125=DIRECTION('ref_axis',(1.,0.,0.));
#10126=DIRECTION('center_axis',(0.,0.,1.));
#10127=DIRECTION('ref_axis',(1.,0.,0.));
#10128=DIRECTION('center_axis',(0.,0.,1.));
#10129=DIRECTION('ref_axis',(1.,0.,0.));
#10130=DIRECTION('center_axis',(0.,0.,1.));
#10131=DIRECTION('ref_axis',(1.,0.,0.));
#10132=DIRECTION('center_axis',(0.,0.,1.));
#10133=DIRECTION('ref_axis',(1.,0.,0.));
#10134=DIRECTION('',(0.,0.,1.));
#10135=DIRECTION('center_axis',(0.,0.,1.));
#10136=DIRECTION('ref_axis',(1.,0.,0.));
#10137=DIRECTION('center_axis',(0.,0.,1.));
#10138=DIRECTION('ref_axis',(1.,0.,0.));
#10139=DIRECTION('',(0.,0.,1.));
#10140=DIRECTION('center_axis',(0.,0.,1.));
#10141=DIRECTION('ref_axis',(1.,0.,0.));
#10142=DIRECTION('center_axis',(0.,0.,1.));
#10143=DIRECTION('ref_axis',(1.,0.,0.));
#10144=DIRECTION('',(0.,0.,1.));
#10145=DIRECTION('center_axis',(0.,0.,1.));
#10146=DIRECTION('ref_axis',(1.,0.,0.));
#10147=DIRECTION('center_axis',(0.,0.,1.));
#10148=DIRECTION('ref_axis',(1.,0.,0.));
#10149=DIRECTION('center_axis',(0.,0.,-1.));
#10150=DIRECTION('ref_axis',(1.,0.,0.));
#10151=DIRECTION('center_axis',(0.,0.,1.));
#10152=DIRECTION('ref_axis',(1.,0.,0.));
#10153=DIRECTION('center_axis',(0.,0.,1.));
#10154=DIRECTION('ref_axis',(1.,0.,0.));
#10155=DIRECTION('',(0.,0.,1.));
#10156=DIRECTION('center_axis',(0.,0.,1.));
#10157=DIRECTION('ref_axis',(1.,0.,0.));
#10158=DIRECTION('center_axis',(0.,0.,1.));
#10159=DIRECTION('ref_axis',(1.,0.,0.));
#10160=DIRECTION('center_axis',(0.,0.,-1.));
#10161=DIRECTION('ref_axis',(1.,0.,0.));
#10162=DIRECTION('center_axis',(0.,0.,1.));
#10163=DIRECTION('ref_axis',(1.,0.,0.));
#10164=DIRECTION('',(0.,0.,1.));
#10165=DIRECTION('center_axis',(0.,0.,-1.));
#10166=DIRECTION('ref_axis',(1.,0.,0.));
#10167=DIRECTION('center_axis',(0.,0.,1.));
#10168=DIRECTION('ref_axis',(1.,0.,0.));
#10169=DIRECTION('',(0.,0.,1.));
#10170=DIRECTION('center_axis',(0.,0.,-1.));
#10171=DIRECTION('ref_axis',(1.,0.,0.));
#10172=DIRECTION('center_axis',(0.,1.,0.));
#10173=DIRECTION('ref_axis',(-1.,0.,0.));
#10174=DIRECTION('',(-1.,0.,0.));
#10175=DIRECTION('',(0.,0.,1.));
#10176=DIRECTION('',(-1.,0.,0.));
#10177=DIRECTION('',(0.,0.,1.));
#10178=DIRECTION('center_axis',(1.,0.,0.));
#10179=DIRECTION('ref_axis',(0.,1.,0.));
#10180=DIRECTION('',(0.,1.,0.));
#10181=DIRECTION('',(0.,1.,0.));
#10182=DIRECTION('',(0.,0.,1.));
#10183=DIRECTION('center_axis',(0.,-1.,0.));
#10184=DIRECTION('ref_axis',(1.,0.,0.));
#10185=DIRECTION('',(1.,0.,0.));
#10186=DIRECTION('',(1.,0.,0.));
#10187=DIRECTION('',(0.,0.,1.));
#10188=DIRECTION('center_axis',(-1.,0.,0.));
#10189=DIRECTION('ref_axis',(0.,-1.,0.));
#10190=DIRECTION('',(0.,-1.,0.));
#10191=DIRECTION('',(0.,-1.,0.));
#10192=DIRECTION('center_axis',(0.,0.,1.));
#10193=DIRECTION('ref_axis',(1.,0.,0.));
#10194=DIRECTION('center_axis',(0.,0.,1.));
#10195=DIRECTION('ref_axis',(1.,0.,0.));
#10196=DIRECTION('axis',(0.,0.,1.));
#10197=DIRECTION('refdir',(1.,0.,0.));
#10198=DIRECTION('center_axis',(0.,1.,0.));
#10199=DIRECTION('ref_axis',(0.,0.,1.));
#10200=DIRECTION('center_axis',(0.,-1.,0.));
#10201=DIRECTION('ref_axis',(1.,0.,0.));
#10202=DIRECTION('center_axis',(0.,-1.,0.));
#10203=DIRECTION('ref_axis',(1.,0.,0.));
#10204=DIRECTION('center_axis',(0.,-1.,0.));
#10205=DIRECTION('ref_axis',(1.,0.,0.));
#10206=DIRECTION('',(0.707106781186548,0.707106781186547,8.65956056235493E-17));
#10207=DIRECTION('center_axis',(0.,-1.,0.));
#10208=DIRECTION('ref_axis',(1.,0.,0.));
#10209=DIRECTION('center_axis',(0.,-1.,0.));
#10210=DIRECTION('ref_axis',(1.,0.,0.));
#10211=DIRECTION('',(0.,1.,0.));
#10212=DIRECTION('center_axis',(0.,1.,0.));
#10213=DIRECTION('ref_axis',(1.,0.,0.));
#10214=DIRECTION('center_axis',(0.,-1.,0.));
#10215=DIRECTION('ref_axis',(1.,0.,0.));
#10216=DIRECTION('',(-0.707106781186547,0.707106781186548,-8.65956056235493E-17));
#10217=DIRECTION('center_axis',(0.,-1.,0.));
#10218=DIRECTION('ref_axis',(0.,0.,-1.));
#10219=DIRECTION('center_axis',(0.,-1.,0.));
#10220=DIRECTION('ref_axis',(1.,0.,0.));
#10221=DIRECTION('center_axis',(0.,1.,0.));
#10222=DIRECTION('ref_axis',(1.,0.,0.));
#10223=DIRECTION('center_axis',(0.,1.,0.));
#10224=DIRECTION('ref_axis',(1.,0.,0.));
#10225=DIRECTION('',(-0.447213595499958,0.894427190999916,-5.47678698264203E-17));
#10226=DIRECTION('center_axis',(0.,-1.,0.));
#10227=DIRECTION('ref_axis',(1.,0.,0.));
#10228=DIRECTION('center_axis',(0.,1.,0.));
#10229=DIRECTION('ref_axis',(1.,0.,0.));
#10230=DIRECTION('',(0.,1.,0.));
#10231=DIRECTION('center_axis',(0.,1.,0.));
#10232=DIRECTION('ref_axis',(1.,0.,0.));
#10233=DIRECTION('center_axis',(0.,-1.,0.));
#10234=DIRECTION('ref_axis',(1.,0.,0.));
#10235=DIRECTION('',(-0.707106781186547,0.707106781186548,-8.65956056235493E-17));
#10236=DIRECTION('center_axis',(0.,-1.,0.));
#10237=DIRECTION('ref_axis',(0.,0.,-1.));
#10238=DIRECTION('center_axis',(0.866025403784439,0.,-0.5));
#10239=DIRECTION('ref_axis',(0.5,0.,0.866025403784439));
#10240=DIRECTION('',(-0.5,0.,-0.866025403784439));
#10241=DIRECTION('',(0.,-1.,0.));
#10242=DIRECTION('',(0.5,0.,0.866025403784439));
#10243=DIRECTION('',(0.,-1.,0.));
#10244=DIRECTION('center_axis',(1.20185167898973E-16,0.,-1.));
#10245=DIRECTION('ref_axis',(1.,0.,1.20185167898973E-16));
#10246=DIRECTION('',(-1.,0.,-1.20185167898973E-16));
#10247=DIRECTION('',(0.,-1.,0.));
#10248=DIRECTION('',(1.,0.,1.20185167898973E-16));
#10249=DIRECTION('center_axis',(-0.866025403784439,0.,-0.5));
#10250=DIRECTION('ref_axis',(0.5,0.,-0.866025403784439));
#10251=DIRECTION('',(-0.5,0.,0.866025403784439));
#10252=DIRECTION('',(0.,-1.,0.));
#10253=DIRECTION('',(0.5,0.,-0.866025403784439));
#10254=DIRECTION('center_axis',(-0.866025403784439,0.,0.5));
#10255=DIRECTION('ref_axis',(-0.5,0.,-0.866025403784439));
#10256=DIRECTION('',(0.5,0.,0.866025403784439));
#10257=DIRECTION('',(0.,-1.,0.));
#10258=DIRECTION('',(-0.5,0.,-0.866025403784439));
#10259=DIRECTION('center_axis',(-2.40370335797945E-16,0.,1.));
#10260=DIRECTION('ref_axis',(-1.,0.,-2.40370335797945E-16));
#10261=DIRECTION('',(1.,0.,2.40370335797945E-16));
#10262=DIRECTION('',(0.,-1.,0.));
#10263=DIRECTION('',(-1.,0.,-2.40370335797945E-16));
#10264=DIRECTION('center_axis',(0.866025403784439,0.,0.5));
#10265=DIRECTION('ref_axis',(-0.5,0.,0.866025403784439));
#10266=DIRECTION('',(0.5,0.,-0.866025403784439));
#10267=DIRECTION('',(-0.5,0.,0.866025403784439));
#10268=DIRECTION('center_axis',(0.,1.,0.));
#10269=DIRECTION('ref_axis',(1.,0.,0.));
#10270=DIRECTION('center_axis',(0.,-1.,0.));
#10271=DIRECTION('ref_axis',(0.,0.,-1.));
#10272=DIRECTION('axis',(0.,0.,1.));
#10273=DIRECTION('refdir',(1.,0.,0.));
#10274=DIRECTION('axis',(0.,0.,1.));
#10275=DIRECTION('refdir',(1.,0.,0.));
#10276=DIRECTION('center_axis',(0.,1.,0.));
#10277=DIRECTION('ref_axis',(1.,0.,0.));
#10278=DIRECTION('center_axis',(0.,1.,0.));
#10279=DIRECTION('ref_axis',(1.,0.,0.));
#10280=DIRECTION('',(0.,1.,0.));
#10281=DIRECTION('center_axis',(0.,-1.,0.));
#10282=DIRECTION('ref_axis',(1.,0.,0.));
#10283=DIRECTION('center_axis',(0.,1.,0.));
#10284=DIRECTION('ref_axis',(1.,0.,0.));
#10285=DIRECTION('center_axis',(0.,1.,0.));
#10286=DIRECTION('ref_axis',(1.,0.,0.));
#10287=DIRECTION('center_axis',(0.,1.,0.));
#10288=DIRECTION('ref_axis',(1.,0.,0.));
#10289=DIRECTION('',(0.5,0.,-0.866025403784439));
#10290=DIRECTION('',(-0.5,0.,-0.866025403784439));
#10291=DIRECTION('',(-1.,0.,-1.60246890531964E-16));
#10292=DIRECTION('',(-0.5,0.,0.866025403784439));
#10293=DIRECTION('',(0.5,0.,0.866025403784439));
#10294=DIRECTION('',(1.,0.,1.60246890531964E-16));
#10295=DIRECTION('center_axis',(0.,-1.,0.));
#10296=DIRECTION('ref_axis',(1.,0.,0.));
#10297=DIRECTION('center_axis',(0.,1.,0.));
#10298=DIRECTION('ref_axis',(1.,0.,0.));
#10299=DIRECTION('',(0.5,0.,-0.866025403784439));
#10300=DIRECTION('',(1.,0.,1.60246890531964E-16));
#10301=DIRECTION('',(0.5,0.,0.866025403784439));
#10302=DIRECTION('',(-0.5,0.,0.866025403784439));
#10303=DIRECTION('',(-1.,0.,-1.60246890531964E-16));
#10304=DIRECTION('',(-0.5,0.,-0.866025403784439));
#10305=DIRECTION('center_axis',(0.,-1.,0.));
#10306=DIRECTION('ref_axis',(1.,0.,0.));
#10307=DIRECTION('center_axis',(-1.60246890531964E-16,0.,1.));
#10308=DIRECTION('ref_axis',(1.,0.,1.60246890531964E-16));
#10309=DIRECTION('',(0.,1.,0.));
#10310=DIRECTION('',(0.,1.,0.));
#10311=DIRECTION('center_axis',(-0.866025403784439,0.,0.5));
#10312=DIRECTION('ref_axis',(0.5,0.,0.866025403784439));
#10313=DIRECTION('',(0.,1.,0.));
#10314=DIRECTION('center_axis',(-0.866025403784439,0.,-0.5));
#10315=DIRECTION('ref_axis',(-0.5,0.,0.866025403784439));
#10316=DIRECTION('',(0.,1.,0.));
#10317=DIRECTION('center_axis',(1.60246890531964E-16,0.,-1.));
#10318=DIRECTION('ref_axis',(-1.,0.,-1.60246890531964E-16));
#10319=DIRECTION('',(0.,1.,0.));
#10320=DIRECTION('center_axis',(0.866025403784439,0.,-0.5));
#10321=DIRECTION('ref_axis',(-0.5,0.,-0.866025403784439));
#10322=DIRECTION('',(0.,1.,0.));
#10323=DIRECTION('center_axis',(0.866025403784439,0.,0.5));
#10324=DIRECTION('ref_axis',(0.5,0.,-0.866025403784439));
#10325=DIRECTION('center_axis',(0.,1.,0.));
#10326=DIRECTION('ref_axis',(0.,0.,1.));
#10327=DIRECTION('center_axis',(0.,-1.,0.));
#10328=DIRECTION('ref_axis',(1.,0.,0.));
#10329=DIRECTION('center_axis',(0.,-1.,0.));
#10330=DIRECTION('ref_axis',(1.,0.,0.));
#10331=DIRECTION('',(0.,1.,0.));
#10332=DIRECTION('center_axis',(0.,-1.,0.));
#10333=DIRECTION('ref_axis',(1.,0.,0.));
#10334=DIRECTION('center_axis',(0.,1.,0.));
#10335=DIRECTION('ref_axis',(0.,0.,1.));
#10336=DIRECTION('center_axis',(0.,-1.,0.));
#10337=DIRECTION('ref_axis',(1.,0.,0.));
#10338=DIRECTION('center_axis',(0.,-1.,0.));
#10339=DIRECTION('ref_axis',(1.,0.,0.));
#10340=DIRECTION('',(0.,1.,0.));
#10341=DIRECTION('center_axis',(0.,-1.,0.));
#10342=DIRECTION('ref_axis',(1.,0.,0.));
#10343=DIRECTION('center_axis',(0.,-1.,0.));
#10344=DIRECTION('ref_axis',(1.,0.,0.));
#10345=DIRECTION('',(0.,1.,0.));
#10346=DIRECTION('center_axis',(0.,-1.,0.));
#10347=DIRECTION('ref_axis',(0.,0.,-1.));
#10348=DIRECTION('center_axis',(0.,-1.,0.));
#10349=DIRECTION('ref_axis',(1.,0.,0.));
#10350=DIRECTION('center_axis',(0.,-1.,0.));
#10351=DIRECTION('ref_axis',(1.,0.,0.));
#10352=DIRECTION('',(0.,1.,0.));
#10353=DIRECTION('axis',(0.,0.,1.));
#10354=DIRECTION('refdir',(1.,0.,0.));
#10355=DIRECTION('center_axis',(0.,1.,0.));
#10356=DIRECTION('ref_axis',(0.,0.,1.));
#10357=DIRECTION('center_axis',(0.,-1.,0.));
#10358=DIRECTION('ref_axis',(1.,0.,0.));
#10359=DIRECTION('center_axis',(0.,-1.,0.));
#10360=DIRECTION('ref_axis',(1.,0.,0.));
#10361=DIRECTION('center_axis',(0.,-1.,0.));
#10362=DIRECTION('ref_axis',(1.,0.,0.));
#10363=DIRECTION('center_axis',(0.,-1.,0.));
#10364=DIRECTION('ref_axis',(1.,0.,0.));
#10365=DIRECTION('',(0.,1.,0.));
#10366=DIRECTION('center_axis',(0.,-1.,0.));
#10367=DIRECTION('ref_axis',(0.,0.,-1.));
#10368=DIRECTION('center_axis',(0.,-1.,0.));
#10369=DIRECTION('ref_axis',(1.,0.,0.));
#10370=DIRECTION('center_axis',(0.,-1.,0.));
#10371=DIRECTION('ref_axis',(1.,0.,0.));
#10372=DIRECTION('center_axis',(0.,-1.,0.));
#10373=DIRECTION('ref_axis',(1.,0.,0.));
#10374=DIRECTION('',(0.,1.,0.));
#10375=DIRECTION('center_axis',(0.,-1.,0.));
#10376=DIRECTION('ref_axis',(0.,0.,-1.));
#10377=DIRECTION('center_axis',(0.,-1.,0.));
#10378=DIRECTION('ref_axis',(1.,0.,0.));
#10379=DIRECTION('center_axis',(0.,-1.,0.));
#10380=DIRECTION('ref_axis',(1.,0.,0.));
#10381=DIRECTION('',(0.,1.,0.));
#10382=DIRECTION('',(0.,0.,1.));
#10383=DIRECTION('',(1.,0.,0.));
#10384=DIRECTION('',(0.,0.,1.));
#10385=DIRECTION('',(1.,0.,0.));
#10386=DIRECTION('axis',(0.,0.,1.));
#10387=DIRECTION('refdir',(1.,0.,0.));
#10388=DIRECTION('center_axis',(0.,-1.,0.));
#10389=DIRECTION('ref_axis',(0.,0.,-1.));
#10390=DIRECTION('center_axis',(-1.,0.,-1.22464679914735E-16));
#10391=DIRECTION('ref_axis',(-1.22464679914735E-16,0.,1.));
#10392=DIRECTION('center_axis',(0.,1.,0.));
#10393=DIRECTION('ref_axis',(0.,0.,-1.));
#10394=DIRECTION('axis',(0.,0.,1.));
#10395=DIRECTION('refdir',(1.,0.,0.));
#10396=DIRECTION('center_axis',(0.,1.,0.));
#10397=DIRECTION('ref_axis',(1.,0.,0.));
#10398=DIRECTION('center_axis',(0.,1.,0.));
#10399=DIRECTION('ref_axis',(1.,0.,0.));
#10400=DIRECTION('',(0.,1.,0.));
#10401=DIRECTION('center_axis',(0.,1.,0.));
#10402=DIRECTION('ref_axis',(1.,0.,0.));
#10403=DIRECTION('center_axis',(0.,1.,0.));
#10404=DIRECTION('ref_axis',(1.,0.,0.));
#10405=DIRECTION('center_axis',(0.,-1.,0.));
#10406=DIRECTION('ref_axis',(1.,0.,0.));
#10407=DIRECTION('center_axis',(0.,1.,0.));
#10408=DIRECTION('ref_axis',(1.,0.,0.));
#10409=DIRECTION('center_axis',(0.,1.,0.));
#10410=DIRECTION('ref_axis',(1.,0.,0.));
#10411=DIRECTION('center_axis',(0.,1.,0.));
#10412=DIRECTION('ref_axis',(1.,0.,0.));
#10413=DIRECTION('',(0.,-1.,0.));
#10414=DIRECTION('center_axis',(0.,-1.,0.));
#10415=DIRECTION('ref_axis',(1.,0.,0.));
#10416=DIRECTION('center_axis',(0.,1.,0.));
#10417=DIRECTION('ref_axis',(1.,0.,0.));
#10418=DIRECTION('center_axis',(0.,-1.,0.));
#10419=DIRECTION('ref_axis',(1.,0.,0.));
#10420=DIRECTION('',(0.,-1.,0.));
#10421=DIRECTION('center_axis',(0.,1.,0.));
#10422=DIRECTION('ref_axis',(1.,0.,0.));
#10423=DIRECTION('center_axis',(0.,1.,0.));
#10424=DIRECTION('ref_axis',(1.,0.,0.));
#10425=DIRECTION('',(0.,-1.,0.));
#10426=DIRECTION('center_axis',(0.,1.,0.));
#10427=DIRECTION('ref_axis',(1.,0.,0.));
#10428=DIRECTION('center_axis',(0.,1.,0.));
#10429=DIRECTION('ref_axis',(1.,0.,0.));
#10430=DIRECTION('center_axis',(0.,1.,0.));
#10431=DIRECTION('ref_axis',(1.,0.,0.));
#10432=DIRECTION('axis',(0.,0.,1.));
#10433=DIRECTION('refdir',(1.,0.,0.));
#10434=DIRECTION('center_axis',(0.,-1.,0.));
#10435=DIRECTION('ref_axis',(0.,0.,-1.));
#10436=DIRECTION('center_axis',(-1.,0.,-1.22464679914735E-16));
#10437=DIRECTION('ref_axis',(-1.22464679914735E-16,0.,1.));
#10438=DIRECTION('center_axis',(0.,1.,0.));
#10439=DIRECTION('ref_axis',(0.,0.,-1.));
#10440=DIRECTION('axis',(0.,0.,1.));
#10441=DIRECTION('refdir',(1.,0.,0.));
#10442=DIRECTION('center_axis',(0.,1.,0.));
#10443=DIRECTION('ref_axis',(1.,0.,0.));
#10444=DIRECTION('center_axis',(0.,1.,0.));
#10445=DIRECTION('ref_axis',(1.,0.,0.));
#10446=DIRECTION('',(0.,-1.,0.));
#10447=DIRECTION('center_axis',(0.,1.,0.));
#10448=DIRECTION('ref_axis',(1.,0.,0.));
#10449=DIRECTION('center_axis',(0.,1.,0.));
#10450=DIRECTION('ref_axis',(1.,0.,0.));
#10451=DIRECTION('center_axis',(0.,1.,0.));
#10452=DIRECTION('ref_axis',(1.,0.,0.));
#10453=DIRECTION('axis',(0.,0.,1.));
#10454=DIRECTION('refdir',(1.,0.,0.));
#10455=DIRECTION('center_axis',(0.,1.,0.));
#10456=DIRECTION('ref_axis',(1.,0.,0.));
#10457=DIRECTION('center_axis',(0.,1.,0.));
#10458=DIRECTION('ref_axis',(1.,0.,0.));
#10459=DIRECTION('',(0.707106781186548,-0.707106781186547,-8.65956056235494E-17));
#10460=DIRECTION('center_axis',(0.,-1.,0.));
#10461=DIRECTION('ref_axis',(1.,0.,0.));
#10462=DIRECTION('center_axis',(0.,1.,0.));
#10463=DIRECTION('ref_axis',(1.,0.,0.));
#10464=DIRECTION('',(0.,-1.,0.));
#10465=DIRECTION('center_axis',(0.,-1.,0.));
#10466=DIRECTION('ref_axis',(1.,0.,0.));
#10467=DIRECTION('center_axis',(0.,1.,0.));
#10468=DIRECTION('ref_axis',(1.,0.,0.));
#10469=DIRECTION('center_axis',(0.,1.,0.));
#10470=DIRECTION('ref_axis',(1.,0.,0.));
#10471=DIRECTION('center_axis',(0.,1.,0.));
#10472=DIRECTION('ref_axis',(1.,0.,0.));
#10473=DIRECTION('',(0.,-1.,0.));
#10474=DIRECTION('center_axis',(0.,1.,0.));
#10475=DIRECTION('ref_axis',(1.,0.,0.));
#10476=DIRECTION('center_axis',(0.,1.,0.));
#10477=DIRECTION('ref_axis',(1.,0.,0.));
#10478=DIRECTION('axis',(0.,0.,1.));
#10479=DIRECTION('refdir',(1.,0.,0.));
#10480=DIRECTION('center_axis',(0.,1.,0.));
#10481=DIRECTION('ref_axis',(1.,0.,0.));
#10482=DIRECTION('',(0.866025403784439,-0.5,1.06057523872491E-16));
#10483=DIRECTION('center_axis',(0.,-1.,0.));
#10484=DIRECTION('ref_axis',(1.,0.,0.));
#10485=DIRECTION('center_axis',(0.,-1.,0.));
#10486=DIRECTION('ref_axis',(1.,0.,0.));
#10487=DIRECTION('center_axis',(0.,1.,0.));
#10488=DIRECTION('ref_axis',(1.,0.,0.));
#10489=DIRECTION('',(-0.866025403784439,-0.5,-1.06057523872491E-16));
#10490=DIRECTION('center_axis',(1.20185167898973E-16,0.,-1.));
#10491=DIRECTION('ref_axis',(-1.,0.,-1.20185167898973E-16));
#10492=DIRECTION('',(0.,1.,0.));
#10493=DIRECTION('',(0.,1.,0.));
#10494=DIRECTION('center_axis',(-0.866025403784439,0.,-0.5));
#10495=DIRECTION('ref_axis',(-0.5,0.,0.866025403784439));
#10496=DIRECTION('',(0.,1.,0.));
#10497=DIRECTION('center_axis',(-0.866025403784439,0.,0.5));
#10498=DIRECTION('ref_axis',(0.5,0.,0.866025403784439));
#10499=DIRECTION('',(0.,1.,0.));
#10500=DIRECTION('center_axis',(0.,1.,0.));
#10501=DIRECTION('ref_axis',(1.,0.,0.));
#10502=DIRECTION('center_axis',(0.,1.,0.));
#10503=DIRECTION('ref_axis',(1.,0.,0.));
#10504=DIRECTION('',(0.,-1.,0.));
#10505=DIRECTION('center_axis',(0.,1.,0.));
#10506=DIRECTION('ref_axis',(1.,0.,0.));
#10507=DIRECTION('center_axis',(-2.40370335797945E-16,0.,1.));
#10508=DIRECTION('ref_axis',(1.,0.,2.40370335797945E-16));
#10509=DIRECTION('',(0.,1.,0.));
#10510=DIRECTION('center_axis',(0.866025403784439,0.,-0.5));
#10511=DIRECTION('ref_axis',(-0.5,0.,-0.866025403784439));
#10512=DIRECTION('',(0.,1.,0.));
#10513=DIRECTION('center_axis',(0.866025403784439,0.,0.5));
#10514=DIRECTION('ref_axis',(0.5,0.,-0.866025403784439));
#10515=DIRECTION('center_axis',(0.,1.,0.));
#10516=DIRECTION('ref_axis',(1.,0.,0.));
#10517=DIRECTION('center_axis',(0.,1.,0.));
#10518=DIRECTION('ref_axis',(1.,0.,0.));
#10519=DIRECTION('axis',(0.,0.,1.));
#10520=DIRECTION('refdir',(1.,0.,0.));
#10521=DIRECTION('center_axis',(0.,0.,1.));
#10522=DIRECTION('ref_axis',(1.,0.,0.));
#10523=DIRECTION('center_axis',(0.,0.,1.));
#10524=DIRECTION('ref_axis',(1.,0.,0.));
#10525=DIRECTION('',(0.,0.,1.));
#10526=DIRECTION('center_axis',(0.,0.,-1.));
#10527=DIRECTION('ref_axis',(1.,0.,0.));
#10528=DIRECTION('center_axis',(0.,0.,1.));
#10529=DIRECTION('ref_axis',(1.,0.,0.));
#10530=DIRECTION('center_axis',(0.,0.,1.));
#10531=DIRECTION('ref_axis',(1.,0.,0.));
#10532=DIRECTION('',(0.,0.,1.));
#10533=DIRECTION('center_axis',(0.,0.,-1.));
#10534=DIRECTION('ref_axis',(1.,0.,0.));
#10535=DIRECTION('center_axis',(0.,0.,1.));
#10536=DIRECTION('ref_axis',(1.,0.,0.));
#10537=DIRECTION('center_axis',(0.,0.,1.));
#10538=DIRECTION('ref_axis',(1.,0.,0.));
#10539=DIRECTION('',(0.,0.,1.));
#10540=DIRECTION('center_axis',(0.,0.,-1.));
#10541=DIRECTION('ref_axis',(1.,0.,0.));
#10542=DIRECTION('center_axis',(0.,0.,1.));
#10543=DIRECTION('ref_axis',(1.,0.,0.));
#10544=DIRECTION('center_axis',(0.,0.,1.));
#10545=DIRECTION('ref_axis',(1.,0.,0.));
#10546=DIRECTION('',(0.,0.,1.));
#10547=DIRECTION('center_axis',(0.,0.,-1.));
#10548=DIRECTION('ref_axis',(1.,0.,0.));
#10549=DIRECTION('center_axis',(0.,0.,1.));
#10550=DIRECTION('ref_axis',(1.,0.,0.));
#10551=DIRECTION('center_axis',(0.,0.,1.));
#10552=DIRECTION('ref_axis',(1.,0.,0.));
#10553=DIRECTION('',(0.,0.,1.));
#10554=DIRECTION('center_axis',(0.,0.,-1.));
#10555=DIRECTION('ref_axis',(1.,0.,0.));
#10556=DIRECTION('center_axis',(0.,0.,1.));
#10557=DIRECTION('ref_axis',(1.,0.,0.));
#10558=DIRECTION('center_axis',(0.,0.,1.));
#10559=DIRECTION('ref_axis',(1.,0.,0.));
#10560=DIRECTION('',(0.,0.,1.));
#10561=DIRECTION('center_axis',(0.,0.,-1.));
#10562=DIRECTION('ref_axis',(1.,0.,0.));
#10563=DIRECTION('center_axis',(0.,0.,1.));
#10564=DIRECTION('ref_axis',(1.,0.,0.));
#10565=DIRECTION('center_axis',(0.,0.,1.));
#10566=DIRECTION('ref_axis',(1.,0.,0.));
#10567=DIRECTION('',(0.,0.,1.));
#10568=DIRECTION('center_axis',(0.,0.,-1.));
#10569=DIRECTION('ref_axis',(1.,0.,0.));
#10570=DIRECTION('center_axis',(0.,0.,1.));
#10571=DIRECTION('ref_axis',(1.,0.,0.));
#10572=DIRECTION('center_axis',(0.,0.,1.));
#10573=DIRECTION('ref_axis',(1.,0.,0.));
#10574=DIRECTION('',(0.,0.,1.));
#10575=DIRECTION('center_axis',(0.,0.,-1.));
#10576=DIRECTION('ref_axis',(1.,0.,0.));
#10577=DIRECTION('center_axis',(0.,1.,0.));
#10578=DIRECTION('ref_axis',(1.,0.,0.));
#10579=DIRECTION('center_axis',(0.,1.,0.));
#10580=DIRECTION('ref_axis',(1.,0.,0.));
#10581=DIRECTION('',(0.,1.,0.));
#10582=DIRECTION('center_axis',(0.,-1.,0.));
#10583=DIRECTION('ref_axis',(1.,0.,0.));
#10584=DIRECTION('center_axis',(0.,1.,0.));
#10585=DIRECTION('ref_axis',(1.,0.,0.));
#10586=DIRECTION('center_axis',(0.,1.,0.));
#10587=DIRECTION('ref_axis',(1.,0.,0.));
#10588=DIRECTION('',(0.,1.,0.));
#10589=DIRECTION('center_axis',(0.,-1.,0.));
#10590=DIRECTION('ref_axis',(1.,0.,0.));
#10591=DIRECTION('center_axis',(0.,1.,0.));
#10592=DIRECTION('ref_axis',(1.,0.,0.));
#10593=DIRECTION('center_axis',(0.,1.,0.));
#10594=DIRECTION('ref_axis',(1.,0.,0.));
#10595=DIRECTION('',(0.,1.,0.));
#10596=DIRECTION('center_axis',(0.,-1.,0.));
#10597=DIRECTION('ref_axis',(1.,0.,0.));
#10598=DIRECTION('center_axis',(0.,1.,0.));
#10599=DIRECTION('ref_axis',(1.,0.,0.));
#10600=DIRECTION('center_axis',(0.,1.,0.));
#10601=DIRECTION('ref_axis',(1.,0.,0.));
#10602=DIRECTION('',(0.,1.,0.));
#10603=DIRECTION('center_axis',(0.,-1.,0.));
#10604=DIRECTION('ref_axis',(1.,0.,0.));
#10605=DIRECTION('center_axis',(0.,1.,0.));
#10606=DIRECTION('ref_axis',(1.,0.,0.));
#10607=DIRECTION('center_axis',(0.,1.,0.));
#10608=DIRECTION('ref_axis',(1.,0.,0.));
#10609=DIRECTION('',(0.,1.,0.));
#10610=DIRECTION('center_axis',(0.,-1.,0.));
#10611=DIRECTION('ref_axis',(1.,0.,0.));
#10612=DIRECTION('center_axis',(-1.,0.,0.));
#10613=DIRECTION('ref_axis',(0.,0.,1.));
#10614=DIRECTION('',(0.,0.,-1.));
#10615=DIRECTION('',(0.,1.,0.));
#10616=DIRECTION('',(0.,0.,1.));
#10617=DIRECTION('',(0.,1.,0.));
#10618=DIRECTION('center_axis',(1.,0.,0.));
#10619=DIRECTION('ref_axis',(0.,0.,-1.));
#10620=DIRECTION('',(0.,0.,1.));
#10621=DIRECTION('',(0.,-1.,0.));
#10622=DIRECTION('',(0.,0.,-1.));
#10623=DIRECTION('',(0.,1.,0.));
#10624=DIRECTION('center_axis',(0.,0.,1.));
#10625=DIRECTION('ref_axis',(1.,0.,0.));
#10626=DIRECTION('',(-1.,0.,0.));
#10627=DIRECTION('',(1.,0.,0.));
#10628=DIRECTION('center_axis',(0.,1.,0.));
#10629=DIRECTION('ref_axis',(0.,0.,1.));
#10630=DIRECTION('',(1.,0.,0.));
#10631=DIRECTION('center_axis',(0.,1.,0.));
#10632=DIRECTION('ref_axis',(1.,0.,0.));
#10633=DIRECTION('',(-1.,0.,0.));
#10634=DIRECTION('center_axis',(0.,1.,0.));
#10635=DIRECTION('ref_axis',(1.,0.,0.));
#10636=DIRECTION('center_axis',(0.,1.,0.));
#10637=DIRECTION('ref_axis',(1.,0.,0.));
#10638=DIRECTION('',(0.,1.,0.));
#10639=DIRECTION('center_axis',(0.,-1.,0.));
#10640=DIRECTION('ref_axis',(1.,0.,0.));
#10641=DIRECTION('center_axis',(0.,1.,0.));
#10642=DIRECTION('ref_axis',(1.,0.,0.));
#10643=DIRECTION('center_axis',(0.,1.,0.));
#10644=DIRECTION('ref_axis',(1.,0.,0.));
#10645=DIRECTION('',(0.,1.,0.));
#10646=DIRECTION('center_axis',(0.,-1.,0.));
#10647=DIRECTION('ref_axis',(1.,0.,0.));
#10648=DIRECTION('center_axis',(0.,1.,0.));
#10649=DIRECTION('ref_axis',(1.,0.,0.));
#10650=DIRECTION('center_axis',(0.,1.,0.));
#10651=DIRECTION('ref_axis',(1.,0.,0.));
#10652=DIRECTION('',(0.,1.,0.));
#10653=DIRECTION('center_axis',(0.,-1.,0.));
#10654=DIRECTION('ref_axis',(1.,0.,0.));
#10655=DIRECTION('center_axis',(0.,1.,0.));
#10656=DIRECTION('ref_axis',(1.,0.,0.));
#10657=DIRECTION('center_axis',(0.,1.,0.));
#10658=DIRECTION('ref_axis',(1.,0.,0.));
#10659=DIRECTION('',(0.,1.,0.));
#10660=DIRECTION('center_axis',(0.,-1.,0.));
#10661=DIRECTION('ref_axis',(1.,0.,0.));
#10662=DIRECTION('center_axis',(0.,1.,0.));
#10663=DIRECTION('ref_axis',(1.,0.,0.));
#10664=DIRECTION('center_axis',(0.,1.,0.));
#10665=DIRECTION('ref_axis',(1.,0.,0.));
#10666=DIRECTION('',(0.,1.,0.));
#10667=DIRECTION('center_axis',(0.,-1.,0.));
#10668=DIRECTION('ref_axis',(1.,0.,0.));
#10669=DIRECTION('center_axis',(-1.,0.,0.));
#10670=DIRECTION('ref_axis',(0.,0.,1.));
#10671=DIRECTION('',(0.,0.,-1.));
#10672=DIRECTION('',(0.,1.,0.));
#10673=DIRECTION('',(0.,0.,1.));
#10674=DIRECTION('',(0.,1.,0.));
#10675=DIRECTION('center_axis',(1.,0.,0.));
#10676=DIRECTION('ref_axis',(0.,0.,-1.));
#10677=DIRECTION('',(0.,0.,1.));
#10678=DIRECTION('',(0.,-1.,0.));
#10679=DIRECTION('',(0.,0.,-1.));
#10680=DIRECTION('',(0.,1.,0.));
#10681=DIRECTION('center_axis',(0.,0.,1.));
#10682=DIRECTION('ref_axis',(1.,0.,0.));
#10683=DIRECTION('',(-1.,0.,0.));
#10684=DIRECTION('',(1.,0.,0.));
#10685=DIRECTION('center_axis',(0.,1.,0.));
#10686=DIRECTION('ref_axis',(0.,0.,1.));
#10687=DIRECTION('',(1.,0.,0.));
#10688=DIRECTION('center_axis',(0.,1.,0.));
#10689=DIRECTION('ref_axis',(1.,0.,0.));
#10690=DIRECTION('',(-1.,0.,0.));
#10691=DIRECTION('center_axis',(0.,1.,0.));
#10692=DIRECTION('ref_axis',(-1.,0.,0.));
#10693=DIRECTION('',(-1.,0.,0.));
#10694=DIRECTION('',(0.,0.,1.));
#10695=DIRECTION('',(-1.,0.,0.));
#10696=DIRECTION('',(0.,0.,1.));
#10697=DIRECTION('center_axis',(1.,0.,0.));
#10698=DIRECTION('ref_axis',(0.,1.,0.));
#10699=DIRECTION('',(0.,1.,0.));
#10700=DIRECTION('',(0.,1.,0.));
#10701=DIRECTION('',(0.,0.,1.));
#10702=DIRECTION('center_axis',(0.,-1.,0.));
#10703=DIRECTION('ref_axis',(1.,0.,0.));
#10704=DIRECTION('',(1.,0.,0.));
#10705=DIRECTION('',(1.,0.,0.));
#10706=DIRECTION('',(0.,0.,1.));
#10707=DIRECTION('center_axis',(-1.,0.,0.));
#10708=DIRECTION('ref_axis',(0.,-1.,0.));
#10709=DIRECTION('',(0.,-1.,0.));
#10710=DIRECTION('',(0.,-1.,0.));
#10711=DIRECTION('center_axis',(0.,0.,1.));
#10712=DIRECTION('ref_axis',(1.,0.,0.));
#10713=DIRECTION('center_axis',(0.,0.,1.));
#10714=DIRECTION('ref_axis',(1.,0.,0.));
#10715=DIRECTION('axis',(0.,0.,1.));
#10716=DIRECTION('refdir',(1.,0.,0.));
#10717=DIRECTION('center_axis',(0.,1.,0.));
#10718=DIRECTION('ref_axis',(1.,0.,0.));
#10719=DIRECTION('center_axis',(0.,1.,0.));
#10720=DIRECTION('ref_axis',(1.,0.,0.));
#10721=DIRECTION('',(0.,1.,0.));
#10722=DIRECTION('center_axis',(0.,-1.,0.));
#10723=DIRECTION('ref_axis',(1.,0.,0.));
#10724=DIRECTION('center_axis',(0.,1.,0.));
#10725=DIRECTION('ref_axis',(1.,0.,0.));
#10726=DIRECTION('center_axis',(0.,1.,0.));
#10727=DIRECTION('ref_axis',(1.,0.,0.));
#10728=DIRECTION('',(0.,1.,0.));
#10729=DIRECTION('center_axis',(0.,-1.,0.));
#10730=DIRECTION('ref_axis',(1.,0.,0.));
#10731=DIRECTION('center_axis',(0.,1.,0.));
#10732=DIRECTION('ref_axis',(1.,0.,0.));
#10733=DIRECTION('center_axis',(0.,1.,0.));
#10734=DIRECTION('ref_axis',(1.,0.,0.));
#10735=DIRECTION('',(0.,1.,0.));
#10736=DIRECTION('center_axis',(0.,-1.,0.));
#10737=DIRECTION('ref_axis',(1.,0.,0.));
#10738=DIRECTION('center_axis',(0.,1.,0.));
#10739=DIRECTION('ref_axis',(1.,0.,0.));
#10740=DIRECTION('center_axis',(0.,1.,0.));
#10741=DIRECTION('ref_axis',(1.,0.,0.));
#10742=DIRECTION('',(0.,1.,0.));
#10743=DIRECTION('center_axis',(0.,-1.,0.));
#10744=DIRECTION('ref_axis',(1.,0.,0.));
#10745=DIRECTION('center_axis',(0.,1.,0.));
#10746=DIRECTION('ref_axis',(1.,0.,0.));
#10747=DIRECTION('center_axis',(0.,-1.,0.));
#10748=DIRECTION('ref_axis',(1.,0.,0.));
#10749=DIRECTION('',(0.,-1.,0.));
#10750=DIRECTION('center_axis',(0.,-1.,0.));
#10751=DIRECTION('ref_axis',(1.,0.,0.));
#10752=DIRECTION('center_axis',(0.,1.,0.));
#10753=DIRECTION('ref_axis',(1.,0.,0.));
#10754=DIRECTION('center_axis',(0.,1.,0.));
#10755=DIRECTION('ref_axis',(1.,0.,0.));
#10756=DIRECTION('',(0.,-1.,0.));
#10757=DIRECTION('center_axis',(0.,1.,0.));
#10758=DIRECTION('ref_axis',(1.,0.,0.));
#10759=DIRECTION('center_axis',(0.,1.,0.));
#10760=DIRECTION('ref_axis',(1.,0.,0.));
#10761=DIRECTION('center_axis',(0.,1.,0.));
#10762=DIRECTION('ref_axis',(1.,0.,0.));
#10763=DIRECTION('axis',(0.,0.,1.));
#10764=DIRECTION('refdir',(1.,0.,0.));
#10765=DIRECTION('center_axis',(0.,1.,0.));
#10766=DIRECTION('ref_axis',(1.,0.,0.));
#10767=DIRECTION('center_axis',(0.,1.,0.));
#10768=DIRECTION('ref_axis',(1.,0.,0.));
#10769=DIRECTION('',(0.,1.,0.));
#10770=DIRECTION('center_axis',(0.,-1.,0.));
#10771=DIRECTION('ref_axis',(1.,0.,0.));
#10772=DIRECTION('center_axis',(0.,1.,0.));
#10773=DIRECTION('ref_axis',(1.,0.,0.));
#10774=DIRECTION('center_axis',(0.,1.,0.));
#10775=DIRECTION('ref_axis',(1.,0.,0.));
#10776=DIRECTION('',(0.,1.,0.));
#10777=DIRECTION('center_axis',(0.,-1.,0.));
#10778=DIRECTION('ref_axis',(1.,0.,0.));
#10779=DIRECTION('center_axis',(0.,1.,0.));
#10780=DIRECTION('ref_axis',(1.,0.,0.));
#10781=DIRECTION('center_axis',(0.,1.,0.));
#10782=DIRECTION('ref_axis',(1.,0.,0.));
#10783=DIRECTION('',(0.,1.,0.));
#10784=DIRECTION('center_axis',(0.,-1.,0.));
#10785=DIRECTION('ref_axis',(1.,0.,0.));
#10786=DIRECTION('center_axis',(0.,1.,0.));
#10787=DIRECTION('ref_axis',(1.,0.,0.));
#10788=DIRECTION('center_axis',(0.,1.,0.));
#10789=DIRECTION('ref_axis',(1.,0.,0.));
#10790=DIRECTION('',(0.,1.,0.));
#10791=DIRECTION('center_axis',(0.,-1.,0.));
#10792=DIRECTION('ref_axis',(1.,0.,0.));
#10793=DIRECTION('center_axis',(0.,1.,0.));
#10794=DIRECTION('ref_axis',(1.,0.,0.));
#10795=DIRECTION('center_axis',(0.,-1.,0.));
#10796=DIRECTION('ref_axis',(1.,0.,0.));
#10797=DIRECTION('',(0.,-1.,0.));
#10798=DIRECTION('center_axis',(0.,-1.,0.));
#10799=DIRECTION('ref_axis',(1.,0.,0.));
#10800=DIRECTION('center_axis',(0.,1.,0.));
#10801=DIRECTION('ref_axis',(1.,0.,0.));
#10802=DIRECTION('center_axis',(0.,1.,0.));
#10803=DIRECTION('ref_axis',(1.,0.,0.));
#10804=DIRECTION('',(0.,-1.,0.));
#10805=DIRECTION('center_axis',(0.,1.,0.));
#10806=DIRECTION('ref_axis',(1.,0.,0.));
#10807=DIRECTION('center_axis',(0.,1.,0.));
#10808=DIRECTION('ref_axis',(1.,0.,0.));
#10809=DIRECTION('center_axis',(0.,1.,0.));
#10810=DIRECTION('ref_axis',(1.,0.,0.));
#10811=DIRECTION('axis',(0.,0.,1.));
#10812=DIRECTION('refdir',(1.,0.,0.));
#10813=DIRECTION('center_axis',(0.,1.,0.));
#10814=DIRECTION('ref_axis',(1.,0.,0.));
#10815=DIRECTION('center_axis',(0.,1.,0.));
#10816=DIRECTION('ref_axis',(1.,0.,0.));
#10817=DIRECTION('',(0.,1.,0.));
#10818=DIRECTION('center_axis',(0.,-1.,0.));
#10819=DIRECTION('ref_axis',(1.,0.,0.));
#10820=DIRECTION('center_axis',(0.,1.,0.));
#10821=DIRECTION('ref_axis',(1.,0.,0.));
#10822=DIRECTION('center_axis',(0.,1.,0.));
#10823=DIRECTION('ref_axis',(1.,0.,0.));
#10824=DIRECTION('',(0.,1.,0.));
#10825=DIRECTION('center_axis',(0.,-1.,0.));
#10826=DIRECTION('ref_axis',(1.,0.,0.));
#10827=DIRECTION('center_axis',(0.,1.,0.));
#10828=DIRECTION('ref_axis',(1.,0.,0.));
#10829=DIRECTION('center_axis',(0.,1.,0.));
#10830=DIRECTION('ref_axis',(1.,0.,0.));
#10831=DIRECTION('',(0.,1.,0.));
#10832=DIRECTION('center_axis',(0.,-1.,0.));
#10833=DIRECTION('ref_axis',(1.,0.,0.));
#10834=DIRECTION('center_axis',(0.,1.,0.));
#10835=DIRECTION('ref_axis',(1.,0.,0.));
#10836=DIRECTION('center_axis',(0.,1.,0.));
#10837=DIRECTION('ref_axis',(1.,0.,0.));
#10838=DIRECTION('',(0.,1.,0.));
#10839=DIRECTION('center_axis',(0.,-1.,0.));
#10840=DIRECTION('ref_axis',(1.,0.,0.));
#10841=DIRECTION('center_axis',(0.,1.,0.));
#10842=DIRECTION('ref_axis',(1.,0.,0.));
#10843=DIRECTION('center_axis',(0.,-1.,0.));
#10844=DIRECTION('ref_axis',(1.,0.,0.));
#10845=DIRECTION('',(0.,-1.,0.));
#10846=DIRECTION('center_axis',(0.,-1.,0.));
#10847=DIRECTION('ref_axis',(1.,0.,0.));
#10848=DIRECTION('center_axis',(0.,1.,0.));
#10849=DIRECTION('ref_axis',(1.,0.,0.));
#10850=DIRECTION('center_axis',(0.,1.,0.));
#10851=DIRECTION('ref_axis',(1.,0.,0.));
#10852=DIRECTION('',(0.,-1.,0.));
#10853=DIRECTION('center_axis',(0.,1.,0.));
#10854=DIRECTION('ref_axis',(1.,0.,0.));
#10855=DIRECTION('center_axis',(0.,1.,0.));
#10856=DIRECTION('ref_axis',(1.,0.,0.));
#10857=DIRECTION('center_axis',(0.,1.,0.));
#10858=DIRECTION('ref_axis',(1.,0.,0.));
#10859=DIRECTION('axis',(0.,0.,1.));
#10860=DIRECTION('refdir',(1.,0.,0.));
#10861=DIRECTION('center_axis',(0.,1.,0.));
#10862=DIRECTION('ref_axis',(1.,0.,0.));
#10863=DIRECTION('center_axis',(0.,1.,0.));
#10864=DIRECTION('ref_axis',(1.,0.,0.));
#10865=DIRECTION('',(0.,1.,0.));
#10866=DIRECTION('center_axis',(0.,-1.,0.));
#10867=DIRECTION('ref_axis',(1.,0.,0.));
#10868=DIRECTION('center_axis',(0.,1.,0.));
#10869=DIRECTION('ref_axis',(1.,0.,0.));
#10870=DIRECTION('center_axis',(0.,1.,0.));
#10871=DIRECTION('ref_axis',(1.,0.,0.));
#10872=DIRECTION('',(0.,1.,0.));
#10873=DIRECTION('center_axis',(0.,-1.,0.));
#10874=DIRECTION('ref_axis',(1.,0.,0.));
#10875=DIRECTION('center_axis',(0.,1.,0.));
#10876=DIRECTION('ref_axis',(1.,0.,0.));
#10877=DIRECTION('center_axis',(0.,1.,0.));
#10878=DIRECTION('ref_axis',(1.,0.,0.));
#10879=DIRECTION('',(0.,1.,0.));
#10880=DIRECTION('center_axis',(0.,-1.,0.));
#10881=DIRECTION('ref_axis',(1.,0.,0.));
#10882=DIRECTION('center_axis',(0.,1.,0.));
#10883=DIRECTION('ref_axis',(1.,0.,0.));
#10884=DIRECTION('center_axis',(0.,1.,0.));
#10885=DIRECTION('ref_axis',(1.,0.,0.));
#10886=DIRECTION('',(0.,1.,0.));
#10887=DIRECTION('center_axis',(0.,-1.,0.));
#10888=DIRECTION('ref_axis',(1.,0.,0.));
#10889=DIRECTION('center_axis',(0.,1.,0.));
#10890=DIRECTION('ref_axis',(1.,0.,0.));
#10891=DIRECTION('center_axis',(0.,-1.,0.));
#10892=DIRECTION('ref_axis',(1.,0.,0.));
#10893=DIRECTION('',(0.,-1.,0.));
#10894=DIRECTION('center_axis',(0.,-1.,0.));
#10895=DIRECTION('ref_axis',(1.,0.,0.));
#10896=DIRECTION('center_axis',(0.,1.,0.));
#10897=DIRECTION('ref_axis',(1.,0.,0.));
#10898=DIRECTION('center_axis',(0.,1.,0.));
#10899=DIRECTION('ref_axis',(1.,0.,0.));
#10900=DIRECTION('',(0.,-1.,0.));
#10901=DIRECTION('center_axis',(0.,1.,0.));
#10902=DIRECTION('ref_axis',(1.,0.,0.));
#10903=DIRECTION('center_axis',(0.,1.,0.));
#10904=DIRECTION('ref_axis',(1.,0.,0.));
#10905=DIRECTION('center_axis',(0.,1.,0.));
#10906=DIRECTION('ref_axis',(1.,0.,0.));
#10907=DIRECTION('axis',(0.,0.,1.));
#10908=DIRECTION('refdir',(1.,0.,0.));
#10909=DIRECTION('axis',(0.,0.,1.));
#10910=DIRECTION('refdir',(1.,0.,0.));
#10911=DIRECTION('center_axis',(0.,1.,0.));
#10912=DIRECTION('ref_axis',(0.,0.,1.));
#10913=DIRECTION('center_axis',(0.,-1.,0.));
#10914=DIRECTION('ref_axis',(1.,0.,0.));
#10915=DIRECTION('',(-1.,0.,0.));
#10916=DIRECTION('',(0.,0.,-1.));
#10917=DIRECTION('',(1.,0.,0.));
#10918=DIRECTION('center_axis',(0.,0.,1.));
#10919=DIRECTION('ref_axis',(1.,0.,0.));
#10920=DIRECTION('',(0.,-1.,0.));
#10921=DIRECTION('',(0.,1.,0.));
#10922=DIRECTION('',(-1.,0.,0.));
#10923=DIRECTION('center_axis',(0.,-1.,0.));
#10924=DIRECTION('ref_axis',(0.,0.,-1.));
#10925=DIRECTION('center_axis',(0.,1.,0.));
#10926=DIRECTION('ref_axis',(1.,0.,0.));
#10927=DIRECTION('',(0.,0.,1.));
#10928=DIRECTION('',(1.,0.,0.));
#10929=DIRECTION('center_axis',(0.,0.,-1.));
#10930=DIRECTION('ref_axis',(-1.,0.,0.));
#10931=DIRECTION('',(0.,1.,0.));
#10932=DIRECTION('',(0.,1.,0.));
#10933=DIRECTION('center_axis',(1.,0.,0.));
#10934=DIRECTION('ref_axis',(0.,0.,-1.));
#10935=DIRECTION('center_axis',(0.,1.,0.));
#10936=DIRECTION('ref_axis',(0.,0.,1.));
#10937=DIRECTION('center_axis',(0.,-1.,0.));
#10938=DIRECTION('ref_axis',(1.,0.,0.));
#10939=DIRECTION('center_axis',(0.,-1.,0.));
#10940=DIRECTION('ref_axis',(1.,0.,0.));
#10941=DIRECTION('center_axis',(0.,-1.,0.));
#10942=DIRECTION('ref_axis',(1.,0.,0.));
#10943=DIRECTION('center_axis',(0.,-1.,0.));
#10944=DIRECTION('ref_axis',(1.,0.,0.));
#10945=DIRECTION('',(0.,1.,0.));
#10946=DIRECTION('center_axis',(0.,-1.,0.));
#10947=DIRECTION('ref_axis',(0.,0.,-1.));
#10948=DIRECTION('center_axis',(0.,-1.,0.));
#10949=DIRECTION('ref_axis',(1.,0.,0.));
#10950=DIRECTION('center_axis',(0.,-1.,0.));
#10951=DIRECTION('ref_axis',(1.,0.,0.));
#10952=DIRECTION('center_axis',(0.,-1.,0.));
#10953=DIRECTION('ref_axis',(1.,0.,0.));
#10954=DIRECTION('',(0.,1.,0.));
#10955=DIRECTION('center_axis',(0.,1.,0.));
#10956=DIRECTION('ref_axis',(0.,0.,1.));
#10957=DIRECTION('center_axis',(0.,-1.,0.));
#10958=DIRECTION('ref_axis',(1.,0.,0.));
#10959=DIRECTION('center_axis',(0.,-1.,0.));
#10960=DIRECTION('ref_axis',(1.,0.,0.));
#10961=DIRECTION('center_axis',(0.,-1.,0.));
#10962=DIRECTION('ref_axis',(1.,0.,0.));
#10963=DIRECTION('',(0.,1.,0.));
#10964=DIRECTION('center_axis',(0.,-1.,0.));
#10965=DIRECTION('ref_axis',(0.,0.,-1.));
#10966=DIRECTION('center_axis',(0.,-1.,0.));
#10967=DIRECTION('ref_axis',(1.,0.,0.));
#10968=DIRECTION('center_axis',(0.,-1.,0.));
#10969=DIRECTION('ref_axis',(1.,0.,0.));
#10970=DIRECTION('center_axis',(0.,-1.,0.));
#10971=DIRECTION('ref_axis',(1.,0.,0.));
#10972=DIRECTION('',(0.,1.,0.));
#10973=DIRECTION('center_axis',(0.,1.,0.));
#10974=DIRECTION('ref_axis',(0.,0.,1.));
#10975=DIRECTION('center_axis',(0.,-1.,0.));
#10976=DIRECTION('ref_axis',(1.,0.,0.));
#10977=DIRECTION('center_axis',(0.,-1.,0.));
#10978=DIRECTION('ref_axis',(1.,0.,0.));
#10979=DIRECTION('center_axis',(0.,-1.,0.));
#10980=DIRECTION('ref_axis',(1.,0.,0.));
#10981=DIRECTION('',(0.,1.,0.));
#10982=DIRECTION('center_axis',(0.,-1.,0.));
#10983=DIRECTION('ref_axis',(0.,0.,-1.));
#10984=DIRECTION('center_axis',(0.,-1.,0.));
#10985=DIRECTION('ref_axis',(1.,0.,0.));
#10986=DIRECTION('center_axis',(0.,-1.,0.));
#10987=DIRECTION('ref_axis',(1.,0.,0.));
#10988=DIRECTION('',(0.,1.,0.));
#10989=DIRECTION('axis',(0.,0.,1.));
#10990=DIRECTION('refdir',(1.,0.,0.));
#10991=DIRECTION('center_axis',(0.,1.,0.));
#10992=DIRECTION('ref_axis',(0.,0.,1.));
#10993=DIRECTION('center_axis',(0.,1.,0.));
#10994=DIRECTION('ref_axis',(1.,0.,0.));
#10995=DIRECTION('',(1.,0.,0.));
#10996=DIRECTION('center_axis',(0.,-1.,0.));
#10997=DIRECTION('ref_axis',(1.,0.,0.));
#10998=DIRECTION('',(-1.,0.,0.));
#10999=DIRECTION('center_axis',(0.,0.,-1.));
#11000=DIRECTION('ref_axis',(-1.,0.,0.));
#11001=DIRECTION('',(0.,-1.,0.));
#11002=DIRECTION('',(0.,1.,0.));
#11003=DIRECTION('',(1.,0.,0.));
#11004=DIRECTION('center_axis',(0.,-1.,0.));
#11005=DIRECTION('ref_axis',(0.,0.,-1.));
#11006=DIRECTION('center_axis',(0.,-1.,0.));
#11007=DIRECTION('ref_axis',(1.,0.,0.));
#11008=DIRECTION('center_axis',(0.,1.,0.));
#11009=DIRECTION('ref_axis',(1.,0.,0.));
#11010=DIRECTION('',(-1.,0.,0.));
#11011=DIRECTION('center_axis',(0.,0.,1.));
#11012=DIRECTION('ref_axis',(1.,0.,0.));
#11013=DIRECTION('',(0.,1.,0.));
#11014=DIRECTION('',(0.,-1.,0.));
#11015=DIRECTION('center_axis',(0.,1.,0.));
#11016=DIRECTION('ref_axis',(0.,0.,1.));
#11017=DIRECTION('center_axis',(0.,-1.,0.));
#11018=DIRECTION('ref_axis',(1.,0.,0.));
#11019=DIRECTION('center_axis',(0.,-1.,0.));
#11020=DIRECTION('ref_axis',(1.,0.,0.));
#11021=DIRECTION('center_axis',(0.,-1.,0.));
#11022=DIRECTION('ref_axis',(1.,0.,0.));
#11023=DIRECTION('center_axis',(0.,-1.,0.));
#11024=DIRECTION('ref_axis',(1.,0.,0.));
#11025=DIRECTION('',(0.,1.,0.));
#11026=DIRECTION('center_axis',(0.,-1.,0.));
#11027=DIRECTION('ref_axis',(0.,0.,-1.));
#11028=DIRECTION('center_axis',(0.,-1.,0.));
#11029=DIRECTION('ref_axis',(1.,0.,0.));
#11030=DIRECTION('center_axis',(0.,-1.,0.));
#11031=DIRECTION('ref_axis',(1.,0.,0.));
#11032=DIRECTION('',(0.,1.,0.));
#11033=DIRECTION('',(0.,0.,1.));
#11034=DIRECTION('',(1.,0.,0.));
#11035=DIRECTION('',(0.,0.,1.));
#11036=DIRECTION('',(1.,0.,0.));
#11037=DIRECTION('axis',(0.,0.,1.));
#11038=DIRECTION('refdir',(1.,0.,0.));
#11039=DIRECTION('center_axis',(0.866025403784439,0.,-0.5));
#11040=DIRECTION('ref_axis',(0.5,0.,0.866025403784439));
#11041=DIRECTION('',(-0.5,0.,-0.866025403784439));
#11042=DIRECTION('',(0.,-1.,0.));
#11043=DIRECTION('',(0.5,0.,0.866025403784439));
#11044=DIRECTION('',(0.,-1.,0.));
#11045=DIRECTION('center_axis',(1.60246890531964E-16,0.,-1.));
#11046=DIRECTION('ref_axis',(1.,0.,1.60246890531964E-16));
#11047=DIRECTION('',(-1.,0.,-1.60246890531964E-16));
#11048=DIRECTION('',(0.,-1.,0.));
#11049=DIRECTION('',(1.,0.,1.60246890531964E-16));
#11050=DIRECTION('center_axis',(-0.866025403784439,0.,-0.5));
#11051=DIRECTION('ref_axis',(0.5,0.,-0.866025403784439));
#11052=DIRECTION('',(-0.5,0.,0.866025403784439));
#11053=DIRECTION('',(0.,-1.,0.));
#11054=DIRECTION('',(0.5,0.,-0.866025403784439));
#11055=DIRECTION('center_axis',(-0.866025403784439,0.,0.5));
#11056=DIRECTION('ref_axis',(-0.5,0.,-0.866025403784439));
#11057=DIRECTION('',(0.5,0.,0.866025403784439));
#11058=DIRECTION('',(0.,-1.,0.));
#11059=DIRECTION('',(-0.5,0.,-0.866025403784439));
#11060=DIRECTION('center_axis',(-1.60246890531964E-16,0.,1.));
#11061=DIRECTION('ref_axis',(-1.,0.,-1.60246890531964E-16));
#11062=DIRECTION('',(1.,0.,1.60246890531964E-16));
#11063=DIRECTION('',(0.,-1.,0.));
#11064=DIRECTION('',(-1.,0.,-1.60246890531964E-16));
#11065=DIRECTION('center_axis',(0.866025403784439,0.,0.5));
#11066=DIRECTION('ref_axis',(-0.5,0.,0.866025403784439));
#11067=DIRECTION('',(0.5,0.,-0.866025403784439));
#11068=DIRECTION('',(-0.5,0.,0.866025403784439));
#11069=DIRECTION('center_axis',(0.,1.,0.));
#11070=DIRECTION('ref_axis',(1.,0.,0.));
#11071=DIRECTION('center_axis',(0.,-1.,0.));
#11072=DIRECTION('ref_axis',(0.,0.,-1.));
#11073=DIRECTION('center_axis',(0.,1.,0.));
#11074=DIRECTION('ref_axis',(1.,0.,0.));
#11075=DIRECTION('center_axis',(0.,1.,0.));
#11076=DIRECTION('ref_axis',(1.,0.,0.));
#11077=DIRECTION('center_axis',(0.,1.,0.));
#11078=DIRECTION('ref_axis',(0.,0.,1.));
#11079=DIRECTION('center_axis',(0.,-1.,0.));
#11080=DIRECTION('ref_axis',(1.,0.,0.));
#11081=DIRECTION('center_axis',(0.,-1.,0.));
#11082=DIRECTION('ref_axis',(1.,0.,0.));
#11083=DIRECTION('center_axis',(0.,-1.,0.));
#11084=DIRECTION('ref_axis',(1.,0.,0.));
#11085=DIRECTION('',(0.707106781186547,0.707106781186548,8.65956056235493E-17));
#11086=DIRECTION('center_axis',(0.,-1.,0.));
#11087=DIRECTION('ref_axis',(1.,0.,0.));
#11088=DIRECTION('center_axis',(0.,-1.,0.));
#11089=DIRECTION('ref_axis',(1.,0.,0.));
#11090=DIRECTION('',(0.,1.,0.));
#11091=DIRECTION('center_axis',(0.,1.,0.));
#11092=DIRECTION('ref_axis',(1.,0.,0.));
#11093=DIRECTION('center_axis',(0.,-1.,0.));
#11094=DIRECTION('ref_axis',(1.,0.,0.));
#11095=DIRECTION('',(-0.707106781186547,0.707106781186548,-8.65956056235493E-17));
#11096=DIRECTION('center_axis',(0.,-1.,0.));
#11097=DIRECTION('ref_axis',(0.,0.,-1.));
#11098=DIRECTION('center_axis',(0.,-1.,0.));
#11099=DIRECTION('ref_axis',(1.,0.,0.));
#11100=DIRECTION('center_axis',(0.,1.,0.));
#11101=DIRECTION('ref_axis',(1.,0.,0.));
#11102=DIRECTION('center_axis',(0.,1.,0.));
#11103=DIRECTION('ref_axis',(1.,0.,0.));
#11104=DIRECTION('',(-0.447213595499958,0.894427190999916,-5.47678698264203E-17));
#11105=DIRECTION('center_axis',(0.,-1.,0.));
#11106=DIRECTION('ref_axis',(1.,0.,0.));
#11107=DIRECTION('',(0.,1.,0.));
#11108=DIRECTION('axis',(0.,0.,1.));
#11109=DIRECTION('refdir',(1.,0.,0.));
#11110=DIRECTION('center_axis',(0.866025403784439,0.,-0.5));
#11111=DIRECTION('ref_axis',(0.5,0.,0.866025403784439));
#11112=DIRECTION('',(-0.5,0.,-0.866025403784439));
#11113=DIRECTION('',(0.,-1.,0.));
#11114=DIRECTION('',(0.5,0.,0.866025403784439));
#11115=DIRECTION('',(0.,-1.,0.));
#11116=DIRECTION('center_axis',(1.20185167898973E-16,0.,-1.));
#11117=DIRECTION('ref_axis',(1.,0.,1.20185167898973E-16));
#11118=DIRECTION('',(-1.,0.,-1.20185167898973E-16));
#11119=DIRECTION('',(0.,-1.,0.));
#11120=DIRECTION('',(1.,0.,1.20185167898973E-16));
#11121=DIRECTION('center_axis',(-0.866025403784439,0.,-0.5));
#11122=DIRECTION('ref_axis',(0.5,0.,-0.866025403784439));
#11123=DIRECTION('',(-0.5,0.,0.866025403784439));
#11124=DIRECTION('',(0.,-1.,0.));
#11125=DIRECTION('',(0.5,0.,-0.866025403784439));
#11126=DIRECTION('center_axis',(-0.866025403784439,0.,0.5));
#11127=DIRECTION('ref_axis',(-0.5,0.,-0.866025403784439));
#11128=DIRECTION('',(0.5,0.,0.866025403784439));
#11129=DIRECTION('',(0.,-1.,0.));
#11130=DIRECTION('',(-0.5,0.,-0.866025403784439));
#11131=DIRECTION('center_axis',(-2.40370335797945E-16,0.,1.));
#11132=DIRECTION('ref_axis',(-1.,0.,-2.40370335797945E-16));
#11133=DIRECTION('',(1.,0.,2.40370335797945E-16));
#11134=DIRECTION('',(0.,-1.,0.));
#11135=DIRECTION('',(-1.,0.,-2.40370335797945E-16));
#11136=DIRECTION('center_axis',(0.866025403784439,0.,0.5));
#11137=DIRECTION('ref_axis',(-0.5,0.,0.866025403784439));
#11138=DIRECTION('',(0.5,0.,-0.866025403784439));
#11139=DIRECTION('',(-0.5,0.,0.866025403784439));
#11140=DIRECTION('center_axis',(0.,1.,0.));
#11141=DIRECTION('ref_axis',(1.,0.,0.));
#11142=DIRECTION('center_axis',(0.,-1.,0.));
#11143=DIRECTION('ref_axis',(0.,0.,-1.));
#11144=DIRECTION('center_axis',(0.,1.,0.));
#11145=DIRECTION('ref_axis',(1.,0.,0.));
#11146=DIRECTION('center_axis',(0.,1.,0.));
#11147=DIRECTION('ref_axis',(1.,0.,0.));
#11148=DIRECTION('center_axis',(0.,1.,0.));
#11149=DIRECTION('ref_axis',(1.,0.,0.));
#11150=DIRECTION('center_axis',(0.,1.,0.));
#11151=DIRECTION('ref_axis',(1.,0.,0.));
#11152=DIRECTION('',(0.,-1.,0.));
#11153=DIRECTION('center_axis',(0.,1.,0.));
#11154=DIRECTION('ref_axis',(1.,0.,0.));
#11155=DIRECTION('center_axis',(0.,1.,0.));
#11156=DIRECTION('ref_axis',(1.,0.,0.));
#11157=DIRECTION('center_axis',(0.,1.,0.));
#11158=DIRECTION('ref_axis',(0.,0.,1.));
#11159=DIRECTION('center_axis',(0.,-1.,0.));
#11160=DIRECTION('ref_axis',(1.,0.,0.));
#11161=DIRECTION('center_axis',(0.,-1.,0.));
#11162=DIRECTION('ref_axis',(1.,0.,0.));
#11163=DIRECTION('center_axis',(0.,-1.,0.));
#11164=DIRECTION('ref_axis',(1.,0.,0.));
#11165=DIRECTION('',(0.707106781186548,0.707106781186547,8.65956056235493E-17));
#11166=DIRECTION('center_axis',(0.,-1.,0.));
#11167=DIRECTION('ref_axis',(1.,0.,0.));
#11168=DIRECTION('center_axis',(0.,-1.,0.));
#11169=DIRECTION('ref_axis',(1.,0.,0.));
#11170=DIRECTION('',(0.,1.,0.));
#11171=DIRECTION('center_axis',(0.,1.,0.));
#11172=DIRECTION('ref_axis',(1.,0.,0.));
#11173=DIRECTION('center_axis',(0.,-1.,0.));
#11174=DIRECTION('ref_axis',(1.,0.,0.));
#11175=DIRECTION('',(-0.707106781186547,0.707106781186548,-8.65956056235493E-17));
#11176=DIRECTION('center_axis',(0.,-1.,0.));
#11177=DIRECTION('ref_axis',(0.,0.,-1.));
#11178=DIRECTION('center_axis',(0.,-1.,0.));
#11179=DIRECTION('ref_axis',(1.,0.,0.));
#11180=DIRECTION('center_axis',(0.,1.,0.));
#11181=DIRECTION('ref_axis',(1.,0.,0.));
#11182=DIRECTION('center_axis',(0.,1.,0.));
#11183=DIRECTION('ref_axis',(1.,0.,0.));
#11184=DIRECTION('',(-0.447213595499958,0.894427190999916,-5.47678698264203E-17));
#11185=DIRECTION('center_axis',(0.,-1.,0.));
#11186=DIRECTION('ref_axis',(1.,0.,0.));
#11187=DIRECTION('center_axis',(0.,1.,0.));
#11188=DIRECTION('ref_axis',(1.,0.,0.));
#11189=DIRECTION('',(0.,1.,0.));
#11190=DIRECTION('center_axis',(0.,1.,0.));
#11191=DIRECTION('ref_axis',(1.,0.,0.));
#11192=DIRECTION('',(-0.707106781186547,0.707106781186548,-8.65956056235493E-17));
#11193=DIRECTION('',(0.,0.,1.));
#11194=DIRECTION('',(1.,0.,0.));
#11195=DIRECTION('',(0.,0.,1.));
#11196=DIRECTION('',(1.,0.,0.));
#11197=DIRECTION('',(0.,0.,1.));
#11198=DIRECTION('',(1.,0.,0.));
#11199=DIRECTION('',(0.,0.,1.));
#11200=DIRECTION('',(1.,0.,0.));
#11201=DIRECTION('',(0.,0.,1.));
#11202=DIRECTION('',(1.,0.,0.));
#11203=DIRECTION('',(0.,0.,1.));
#11204=DIRECTION('',(1.,0.,0.));
#11205=DIRECTION('',(0.,0.,1.));
#11206=DIRECTION('',(1.,0.,0.));
#11207=DIRECTION('',(0.,0.,1.));
#11208=DIRECTION('',(1.,0.,0.));
#11209=DIRECTION('',(0.,0.,1.));
#11210=DIRECTION('',(1.,0.,0.));
#11211=DIRECTION('',(0.,0.,1.));
#11212=DIRECTION('',(1.,0.,0.));
#11213=DIRECTION('',(0.,1.,2.22044604925031E-16));
#11214=DIRECTION('',(1.,0.,0.));
#11215=DIRECTION('',(0.,1.,2.22044604925031E-16));
#11216=DIRECTION('',(1.,0.,0.));
#11217=DIRECTION('',(0.,0.,1.));
#11218=DIRECTION('',(2.22044604925031E-16,-1.,0.));
#11219=DIRECTION('',(0.,-1.,2.22044604925031E-16));
#11220=DIRECTION('',(1.,0.,0.));
#11221=DIRECTION('',(0.,0.,1.));
#11222=DIRECTION('',(-1.,1.22464679914735E-16,0.));
#11223=DIRECTION('',(0.,1.,2.22044604925031E-16));
#11224=DIRECTION('',(1.,0.,0.));
#11225=DIRECTION('',(0.,1.,2.22044604925031E-16));
#11226=DIRECTION('',(1.,0.,0.));
#11227=DIRECTION('',(0.,0.,1.));
#11228=DIRECTION('',(2.22044604925031E-16,-1.,0.));
#11229=DIRECTION('',(0.,-1.,2.22044604925031E-16));
#11230=DIRECTION('',(1.,0.,0.));
#11231=DIRECTION('',(0.,0.,1.));
#11232=DIRECTION('',(1.,0.,0.));
#11233=DIRECTION('',(0.,0.,1.));
#11234=DIRECTION('',(1.,0.,0.));
#11235=DIRECTION('',(0.,0.,1.));
#11236=DIRECTION('',(1.,0.,0.));
#11237=DIRECTION('',(0.,0.,1.));
#11238=DIRECTION('',(-1.,1.22464679914735E-16,0.));
#11239=DIRECTION('',(0.,0.,1.));
#11240=DIRECTION('',(1.,0.,0.));
#11241=DIRECTION('',(0.,0.,1.));
#11242=DIRECTION('',(1.,0.,0.));
#11243=DIRECTION('',(0.,0.,1.));
#11244=DIRECTION('',(1.,0.,0.));
#11245=DIRECTION('',(0.,0.,1.));
#11246=DIRECTION('',(1.,0.,0.));
#11247=DIRECTION('',(0.,0.,1.));
#11248=DIRECTION('',(-1.,1.22464679914735E-16,0.));
#11249=DIRECTION('',(0.,0.,1.));
#11250=DIRECTION('',(1.,0.,0.));
#11251=DIRECTION('',(0.,0.,1.));
#11252=DIRECTION('',(1.,0.,0.));
#11253=DIRECTION('',(0.,0.,1.));
#11254=DIRECTION('',(1.,0.,0.));
#11255=DIRECTION('',(0.,0.,1.));
#11256=DIRECTION('',(1.,0.,0.));
#11257=DIRECTION('',(0.,0.,1.));
#11258=DIRECTION('',(-1.,1.22464679914735E-16,0.));
#11259=DIRECTION('',(0.,0.,1.));
#11260=DIRECTION('',(1.,0.,0.));
#11261=DIRECTION('',(0.,0.,1.));
#11262=DIRECTION('',(1.,0.,0.));
#11263=DIRECTION('',(0.,0.,1.));
#11264=DIRECTION('',(1.,0.,0.));
#11265=DIRECTION('',(0.,0.,1.));
#11266=DIRECTION('',(1.,0.,0.));
#11267=DIRECTION('',(0.,0.,1.));
#11268=DIRECTION('',(-1.,1.22464679914735E-16,0.));
#11269=DIRECTION('',(0.,0.,1.));
#11270=DIRECTION('',(1.,0.,0.));
#11271=DIRECTION('',(0.,0.,1.));
#11272=DIRECTION('',(1.,0.,0.));
#11273=DIRECTION('',(0.,0.,1.));
#11274=DIRECTION('',(1.,0.,0.));
#11275=DIRECTION('',(0.,0.,1.));
#11276=DIRECTION('',(1.,0.,0.));
#11277=DIRECTION('',(0.,0.,1.));
#11278=DIRECTION('',(1.,0.,0.));
#11279=DIRECTION('',(0.,0.,1.));
#11280=DIRECTION('',(1.,0.,0.));
#11281=DIRECTION('',(0.,0.,1.));
#11282=DIRECTION('',(1.,0.,0.));
#11283=DIRECTION('',(0.,0.,1.));
#11284=DIRECTION('',(1.,0.,0.));
#11285=DIRECTION('',(0.,0.,1.));
#11286=DIRECTION('',(1.,0.,0.));
#11287=DIRECTION('',(0.,0.,1.));
#11288=DIRECTION('',(-1.,1.22464679914735E-16,0.));
#11289=DIRECTION('',(0.,0.,1.));
#11290=DIRECTION('',(-1.,1.22464679914735E-16,0.));
#11291=DIRECTION('',(0.,0.,1.));
#11292=DIRECTION('',(-1.,1.22464679914735E-16,0.));
#11293=DIRECTION('',(0.,0.,1.));
#11294=DIRECTION('',(-1.,1.22464679914735E-16,0.));
#11295=DIRECTION('',(0.,0.,1.));
#11296=DIRECTION('',(1.,0.,0.));
#11297=DIRECTION('',(0.,0.,1.));
#11298=DIRECTION('',(1.,0.,0.));
#11299=DIRECTION('',(0.,0.,1.));
#11300=DIRECTION('',(1.,0.,0.));
#11301=DIRECTION('',(0.,0.,1.));
#11302=DIRECTION('',(1.,0.,0.));
#11303=DIRECTION('',(0.,0.,1.));
#11304=DIRECTION('',(1.,0.,0.));
#11305=DIRECTION('',(0.,0.,1.));
#11306=DIRECTION('',(-1.,1.22464679914735E-16,0.));
#11307=DIRECTION('',(0.,0.,1.));
#11308=DIRECTION('',(-1.,1.22464679914735E-16,0.));
#11309=DIRECTION('',(0.,0.,1.));
#11310=DIRECTION('',(-1.,1.22464679914735E-16,0.));
#11311=DIRECTION('',(0.,0.,1.));
#11312=DIRECTION('',(-1.,1.22464679914735E-16,0.));
#11313=DIRECTION('',(0.,0.,1.));
#11314=DIRECTION('',(1.,0.,0.));
#11315=DIRECTION('',(0.,0.,1.));
#11316=DIRECTION('',(1.,0.,0.));
#11317=DIRECTION('',(0.,0.,1.));
#11318=DIRECTION('',(1.,0.,0.));
#11319=DIRECTION('',(0.,0.,1.));
#11320=DIRECTION('',(1.,0.,0.));
#11321=DIRECTION('',(0.,-1.,2.22044604925031E-16));
#11322=DIRECTION('',(1.,0.,0.));
#11323=DIRECTION('',(0.,-1.,2.22044604925031E-16));
#11324=DIRECTION('',(1.,0.,0.));
#11325=DIRECTION('',(0.,-1.,2.22044604925031E-16));
#11326=DIRECTION('',(1.,0.,0.));
#11327=DIRECTION('',(0.,-1.,2.22044604925031E-16));
#11328=DIRECTION('',(1.,0.,0.));
#11329=DIRECTION('axis',(0.,0.,1.));
#11330=DIRECTION('refdir',(1.,0.,0.));
#11331=DIRECTION('axis',(0.,0.,1.));
#11332=DIRECTION('refdir',(1.,0.,0.));
#11333=DIRECTION('center_axis',(0.,1.,0.));
#11334=DIRECTION('ref_axis',(1.,0.,0.));
#11335=DIRECTION('center_axis',(0.,1.,0.));
#11336=DIRECTION('ref_axis',(1.,0.,0.));
#11337=DIRECTION('',(0.,1.,0.));
#11338=DIRECTION('center_axis',(0.,-1.,0.));
#11339=DIRECTION('ref_axis',(1.,0.,0.));
#11340=DIRECTION('center_axis',(0.,1.,0.));
#11341=DIRECTION('ref_axis',(1.,0.,0.));
#11342=DIRECTION('center_axis',(0.,1.,0.));
#11343=DIRECTION('ref_axis',(1.,0.,0.));
#11344=DIRECTION('center_axis',(0.,1.,0.));
#11345=DIRECTION('ref_axis',(1.,0.,0.));
#11346=DIRECTION('center_axis',(0.,-1.,0.));
#11347=DIRECTION('ref_axis',(1.,0.,0.));
#11348=DIRECTION('',(0.,1.,0.));
#11349=DIRECTION('center_axis',(0.,-1.,0.));
#11350=DIRECTION('ref_axis',(1.,0.,0.));
#11351=DIRECTION('center_axis',(0.,1.,0.));
#11352=DIRECTION('ref_axis',(1.,0.,0.));
#11353=DIRECTION('center_axis',(0.,1.,0.));
#11354=DIRECTION('ref_axis',(1.,0.,0.));
#11355=DIRECTION('center_axis',(0.,1.,0.));
#11356=DIRECTION('ref_axis',(1.,0.,0.));
#11357=DIRECTION('center_axis',(0.,-1.,0.));
#11358=DIRECTION('ref_axis',(1.,0.,0.));
#11359=DIRECTION('center_axis',(0.,1.,0.));
#11360=DIRECTION('ref_axis',(1.,0.,0.));
#11361=DIRECTION('',(0.,-1.,0.));
#11362=DIRECTION('center_axis',(0.,1.,0.));
#11363=DIRECTION('ref_axis',(1.,0.,0.));
#11364=DIRECTION('center_axis',(0.,1.,0.));
#11365=DIRECTION('ref_axis',(1.,0.,0.));
#11366=DIRECTION('',(0.,-1.,0.));
#11367=DIRECTION('center_axis',(0.,-1.,0.));
#11368=DIRECTION('ref_axis',(1.,0.,0.));
#11369=DIRECTION('center_axis',(0.,1.,0.));
#11370=DIRECTION('ref_axis',(1.,0.,0.));
#11371=DIRECTION('center_axis',(0.,1.,0.));
#11372=DIRECTION('ref_axis',(1.,0.,0.));
#11373=DIRECTION('',(0.,-1.,0.));
#11374=DIRECTION('center_axis',(0.,1.,0.));
#11375=DIRECTION('ref_axis',(1.,0.,0.));
#11376=DIRECTION('center_axis',(0.,1.,0.));
#11377=DIRECTION('ref_axis',(1.,0.,0.));
#11378=DIRECTION('axis',(0.,0.,1.));
#11379=DIRECTION('refdir',(1.,0.,0.));
#11380=DIRECTION('center_axis',(0.,-1.,0.));
#11381=DIRECTION('ref_axis',(0.,0.,-1.));
#11382=DIRECTION('center_axis',(-1.,0.,-1.22464679914735E-16));
#11383=DIRECTION('ref_axis',(-1.22464679914735E-16,0.,1.));
#11384=DIRECTION('center_axis',(0.,1.,0.));
#11385=DIRECTION('ref_axis',(0.,0.,-1.));
#11386=DIRECTION('axis',(0.,0.,1.));
#11387=DIRECTION('refdir',(1.,0.,0.));
#11388=DIRECTION('center_axis',(0.,1.,0.));
#11389=DIRECTION('ref_axis',(1.,0.,0.));
#11390=DIRECTION('center_axis',(0.,1.,0.));
#11391=DIRECTION('ref_axis',(1.,0.,0.));
#11392=DIRECTION('',(0.,1.,0.));
#11393=DIRECTION('center_axis',(0.,-1.,0.));
#11394=DIRECTION('ref_axis',(1.,0.,0.));
#11395=DIRECTION('center_axis',(0.,1.,0.));
#11396=DIRECTION('ref_axis',(1.,0.,0.));
#11397=DIRECTION('center_axis',(0.,1.,0.));
#11398=DIRECTION('ref_axis',(1.,0.,0.));
#11399=DIRECTION('center_axis',(0.,1.,0.));
#11400=DIRECTION('ref_axis',(1.,0.,0.));
#11401=DIRECTION('',(0.,-1.,0.));
#11402=DIRECTION('center_axis',(0.,1.,0.));
#11403=DIRECTION('ref_axis',(1.,0.,0.));
#11404=DIRECTION('center_axis',(0.,1.,0.));
#11405=DIRECTION('ref_axis',(1.,0.,0.));
#11406=DIRECTION('center_axis',(0.,1.,0.));
#11407=DIRECTION('ref_axis',(1.,0.,0.));
#11408=DIRECTION('axis',(0.,0.,1.));
#11409=DIRECTION('refdir',(1.,0.,0.));
#11410=DIRECTION('center_axis',(0.,1.,0.));
#11411=DIRECTION('ref_axis',(0.,0.,1.));
#11412=DIRECTION('center_axis',(0.,-1.,0.));
#11413=DIRECTION('ref_axis',(1.,0.,0.));
#11414=DIRECTION('center_axis',(0.,-1.,0.));
#11415=DIRECTION('ref_axis',(1.,0.,0.));
#11416=DIRECTION('center_axis',(0.,-1.,0.));
#11417=DIRECTION('ref_axis',(1.,0.,0.));
#11418=DIRECTION('',(0.707106781186547,0.707106781186548,8.65956056235493E-17));
#11419=DIRECTION('center_axis',(0.,-1.,0.));
#11420=DIRECTION('ref_axis',(1.,0.,0.));
#11421=DIRECTION('center_axis',(0.,-1.,0.));
#11422=DIRECTION('ref_axis',(1.,0.,0.));
#11423=DIRECTION('',(0.,1.,0.));
#11424=DIRECTION('center_axis',(0.,1.,0.));
#11425=DIRECTION('ref_axis',(1.,0.,0.));
#11426=DIRECTION('center_axis',(0.,-1.,0.));
#11427=DIRECTION('ref_axis',(1.,0.,0.));
#11428=DIRECTION('',(-0.707106781186547,0.707106781186548,-8.65956056235493E-17));
#11429=DIRECTION('center_axis',(0.,-1.,0.));
#11430=DIRECTION('ref_axis',(0.,0.,-1.));
#11431=DIRECTION('center_axis',(0.,-1.,0.));
#11432=DIRECTION('ref_axis',(1.,0.,0.));
#11433=DIRECTION('center_axis',(0.,1.,0.));
#11434=DIRECTION('ref_axis',(1.,0.,0.));
#11435=DIRECTION('center_axis',(0.,1.,0.));
#11436=DIRECTION('ref_axis',(1.,0.,0.));
#11437=DIRECTION('',(-0.447213595499958,0.894427190999916,-5.47678698264203E-17));
#11438=DIRECTION('center_axis',(0.,-1.,0.));
#11439=DIRECTION('ref_axis',(1.,0.,0.));
#11440=DIRECTION('center_axis',(0.,1.,0.));
#11441=DIRECTION('ref_axis',(1.,0.,0.));
#11442=DIRECTION('',(0.,1.,0.));
#11443=DIRECTION('center_axis',(0.,1.,0.));
#11444=DIRECTION('ref_axis',(1.,0.,0.));
#11445=DIRECTION('center_axis',(0.,-1.,0.));
#11446=DIRECTION('ref_axis',(1.,0.,0.));
#11447=DIRECTION('',(-0.707106781186547,0.707106781186548,-8.65956056235493E-17));
#11448=DIRECTION('center_axis',(0.,-1.,0.));
#11449=DIRECTION('ref_axis',(0.,0.,-1.));
#11450=DIRECTION('center_axis',(0.866025403784439,0.,-0.5));
#11451=DIRECTION('ref_axis',(0.5,0.,0.866025403784439));
#11452=DIRECTION('',(-0.5,0.,-0.866025403784439));
#11453=DIRECTION('',(0.,-1.,0.));
#11454=DIRECTION('',(0.5,0.,0.866025403784439));
#11455=DIRECTION('',(0.,-1.,0.));
#11456=DIRECTION('center_axis',(1.60246890531964E-16,0.,-1.));
#11457=DIRECTION('ref_axis',(1.,0.,1.60246890531964E-16));
#11458=DIRECTION('',(-1.,0.,-1.60246890531964E-16));
#11459=DIRECTION('',(0.,-1.,0.));
#11460=DIRECTION('',(1.,0.,1.60246890531964E-16));
#11461=DIRECTION('center_axis',(-0.866025403784439,0.,-0.5));
#11462=DIRECTION('ref_axis',(0.5,0.,-0.866025403784439));
#11463=DIRECTION('',(-0.5,0.,0.866025403784439));
#11464=DIRECTION('',(0.,-1.,0.));
#11465=DIRECTION('',(0.5,0.,-0.866025403784439));
#11466=DIRECTION('center_axis',(-0.866025403784439,0.,0.5));
#11467=DIRECTION('ref_axis',(-0.5,0.,-0.866025403784439));
#11468=DIRECTION('',(0.5,0.,0.866025403784439));
#11469=DIRECTION('',(0.,-1.,0.));
#11470=DIRECTION('',(-0.5,0.,-0.866025403784439));
#11471=DIRECTION('center_axis',(-1.60246890531964E-16,0.,1.));
#11472=DIRECTION('ref_axis',(-1.,0.,-1.60246890531964E-16));
#11473=DIRECTION('',(1.,0.,1.60246890531964E-16));
#11474=DIRECTION('',(0.,-1.,0.));
#11475=DIRECTION('',(-1.,0.,-1.60246890531964E-16));
#11476=DIRECTION('center_axis',(0.866025403784439,0.,0.5));
#11477=DIRECTION('ref_axis',(-0.5,0.,0.866025403784439));
#11478=DIRECTION('',(0.5,0.,-0.866025403784439));
#11479=DIRECTION('',(-0.5,0.,0.866025403784439));
#11480=DIRECTION('center_axis',(0.,1.,0.));
#11481=DIRECTION('ref_axis',(1.,0.,0.));
#11482=DIRECTION('center_axis',(0.,-1.,0.));
#11483=DIRECTION('ref_axis',(0.,0.,-1.));
#11484=DIRECTION('axis',(0.,0.,1.));
#11485=DIRECTION('refdir',(1.,0.,0.));
#11486=DIRECTION('center_axis',(1.,0.,0.));
#11487=DIRECTION('ref_axis',(0.,0.,-1.));
#11488=DIRECTION('center_axis',(1.,0.,0.));
#11489=DIRECTION('ref_axis',(0.,0.,-1.));
#11490=DIRECTION('',(1.,0.,0.));
#11491=DIRECTION('center_axis',(-1.,0.,0.));
#11492=DIRECTION('ref_axis',(0.,0.,-1.));
#11493=DIRECTION('center_axis',(1.,0.,0.));
#11494=DIRECTION('ref_axis',(0.,0.,-1.));
#11495=DIRECTION('center_axis',(1.,0.,0.));
#11496=DIRECTION('ref_axis',(0.,0.,-1.));
#11497=DIRECTION('',(1.,0.,0.));
#11498=DIRECTION('center_axis',(-1.,0.,0.));
#11499=DIRECTION('ref_axis',(0.,0.,-1.));
#11500=DIRECTION('center_axis',(0.,0.,1.));
#11501=DIRECTION('ref_axis',(1.,0.,0.));
#11502=DIRECTION('',(0.,1.,0.));
#11503=DIRECTION('center_axis',(0.,0.,1.));
#11504=DIRECTION('ref_axis',(1.,0.,0.));
#11505=DIRECTION('center_axis',(0.,0.,1.));
#11506=DIRECTION('ref_axis',(1.,0.,0.));
#11507=DIRECTION('center_axis',(0.,0.,1.));
#11508=DIRECTION('ref_axis',(1.,0.,0.));
#11509=DIRECTION('',(0.,0.,1.));
#11510=DIRECTION('center_axis',(0.,0.,-1.));
#11511=DIRECTION('ref_axis',(1.,0.,0.));
#11512=DIRECTION('center_axis',(0.,0.,1.));
#11513=DIRECTION('ref_axis',(1.,0.,0.));
#11514=DIRECTION('center_axis',(0.,0.,1.));
#11515=DIRECTION('ref_axis',(1.,0.,0.));
#11516=DIRECTION('',(0.,-1.,0.));
#11517=DIRECTION('center_axis',(0.,1.,0.));
#11518=DIRECTION('ref_axis',(1.,0.,0.));
#11519=DIRECTION('center_axis',(0.,1.,0.));
#11520=DIRECTION('ref_axis',(1.,0.,0.));
#11521=DIRECTION('',(0.,1.,0.));
#11522=DIRECTION('center_axis',(0.,-1.,0.));
#11523=DIRECTION('ref_axis',(1.,0.,0.));
#11524=DIRECTION('center_axis',(1.,0.,0.));
#11525=DIRECTION('ref_axis',(0.,1.,0.));
#11526=DIRECTION('',(0.,-1.,0.));
#11527=DIRECTION('',(0.,0.,1.));
#11528=DIRECTION('',(0.,1.,0.));
#11529=DIRECTION('',(0.,0.,-1.));
#11530=DIRECTION('center_axis',(0.,1.,0.));
#11531=DIRECTION('ref_axis',(-1.,0.,0.));
#11532=DIRECTION('',(1.,0.,0.));
#11533=DIRECTION('',(0.,0.,1.));
#11534=DIRECTION('',(-1.,0.,0.));
#11535=DIRECTION('center_axis',(-1.,0.,0.));
#11536=DIRECTION('ref_axis',(0.,-1.,0.));
#11537=DIRECTION('',(0.,1.,0.));
#11538=DIRECTION('',(0.,0.,1.));
#11539=DIRECTION('',(0.,-1.,0.));
#11540=DIRECTION('center_axis',(0.,0.,1.));
#11541=DIRECTION('ref_axis',(1.,0.,0.));
#11542=DIRECTION('',(1.,0.,0.));
#11543=DIRECTION('',(0.,-1.,0.));
#11544=DIRECTION('',(-1.,0.,0.));
#11545=DIRECTION('',(0.,1.,0.));
#11546=DIRECTION('',(1.,0.,0.));
#11547=DIRECTION('center_axis',(0.,-1.,0.));
#11548=DIRECTION('ref_axis',(1.,0.,0.));
#11549=DIRECTION('',(1.,0.,0.));
#11550=DIRECTION('',(0.,0.,1.));
#11551=DIRECTION('center_axis',(0.,-1.,0.));
#11552=DIRECTION('ref_axis',(1.,0.,0.));
#11553=DIRECTION('',(0.,0.,1.));
#11554=DIRECTION('',(1.,0.,0.));
#11555=DIRECTION('center_axis',(0.,1.,0.));
#11556=DIRECTION('ref_axis',(-1.,0.,0.));
#11557=DIRECTION('',(0.,0.,1.));
#11558=DIRECTION('',(-1.,0.,0.));
#11559=DIRECTION('',(0.,0.,1.));
#11560=DIRECTION('center_axis',(1.,0.,0.));
#11561=DIRECTION('ref_axis',(0.,1.,0.));
#11562=DIRECTION('',(0.,1.,0.));
#11563=DIRECTION('center_axis',(-1.,0.,0.));
#11564=DIRECTION('ref_axis',(0.,-1.,0.));
#11565=DIRECTION('',(0.,-1.,0.));
#11566=DIRECTION('center_axis',(0.,0.,1.));
#11567=DIRECTION('ref_axis',(1.,0.,0.));
#11568=DIRECTION('axis',(0.,0.,1.));
#11569=DIRECTION('refdir',(1.,0.,0.));
#11570=DIRECTION('center_axis',(0.866025403784439,0.,-0.5));
#11571=DIRECTION('ref_axis',(0.5,0.,0.866025403784439));
#11572=DIRECTION('',(0.5,0.,0.866025403784439));
#11573=DIRECTION('',(0.,-1.,0.));
#11574=DIRECTION('',(0.5,0.,0.866025403784439));
#11575=DIRECTION('',(0.,-1.,0.));
#11576=DIRECTION('center_axis',(1.20185167898973E-16,0.,-1.));
#11577=DIRECTION('ref_axis',(1.,0.,1.20185167898973E-16));
#11578=DIRECTION('',(1.,0.,1.20185167898973E-16));
#11579=DIRECTION('',(0.,-1.,0.));
#11580=DIRECTION('',(1.,0.,1.20185167898973E-16));
#11581=DIRECTION('center_axis',(-0.866025403784439,0.,-0.5));
#11582=DIRECTION('ref_axis',(0.5,0.,-0.866025403784439));
#11583=DIRECTION('',(0.5,0.,-0.866025403784439));
#11584=DIRECTION('',(0.,-1.,0.));
#11585=DIRECTION('',(0.5,0.,-0.866025403784439));
#11586=DIRECTION('center_axis',(-0.866025403784439,0.,0.5));
#11587=DIRECTION('ref_axis',(-0.5,0.,-0.866025403784439));
#11588=DIRECTION('',(-0.5,0.,-0.866025403784439));
#11589=DIRECTION('',(0.,-1.,0.));
#11590=DIRECTION('',(-0.5,0.,-0.866025403784439));
#11591=DIRECTION('center_axis',(-2.40370335797945E-16,0.,1.));
#11592=DIRECTION('ref_axis',(-1.,0.,-2.40370335797945E-16));
#11593=DIRECTION('',(-1.,0.,-2.40370335797945E-16));
#11594=DIRECTION('',(0.,-1.,0.));
#11595=DIRECTION('',(-1.,0.,-2.40370335797945E-16));
#11596=DIRECTION('center_axis',(0.866025403784439,0.,0.5));
#11597=DIRECTION('ref_axis',(-0.5,0.,0.866025403784439));
#11598=DIRECTION('',(-0.5,0.,0.866025403784439));
#11599=DIRECTION('',(-0.5,0.,0.866025403784439));
#11600=DIRECTION('center_axis',(0.,-1.,0.));
#11601=DIRECTION('ref_axis',(0.,0.,-1.));
#11602=DIRECTION('center_axis',(0.,1.,0.));
#11603=DIRECTION('ref_axis',(0.,0.,1.));
#11604=DIRECTION('center_axis',(0.,-1.,0.));
#11605=DIRECTION('ref_axis',(1.,0.,0.));
#11606=DIRECTION('center_axis',(0.,-1.,0.));
#11607=DIRECTION('ref_axis',(1.,0.,0.));
#11608=DIRECTION('center_axis',(0.,-1.,0.));
#11609=DIRECTION('ref_axis',(1.,0.,0.));
#11610=DIRECTION('',(0.707106781186548,0.707106781186547,8.65956056235494E-17));
#11611=DIRECTION('center_axis',(0.,-1.,0.));
#11612=DIRECTION('ref_axis',(1.,0.,0.));
#11613=DIRECTION('center_axis',(0.,1.,0.));
#11614=DIRECTION('ref_axis',(1.,0.,0.));
#11615=DIRECTION('',(0.,1.,0.));
#11616=DIRECTION('center_axis',(0.,1.,0.));
#11617=DIRECTION('ref_axis',(1.,0.,0.));
#11618=DIRECTION('center_axis',(0.,-1.,0.));
#11619=DIRECTION('ref_axis',(1.,0.,0.));
#11620=DIRECTION('',(-0.707106781186548,0.707106781186547,-8.65956056235494E-17));
#11621=DIRECTION('center_axis',(0.,-1.,0.));
#11622=DIRECTION('ref_axis',(0.,0.,-1.));
#11623=DIRECTION('axis',(0.,0.,1.));
#11624=DIRECTION('refdir',(1.,0.,0.));
#11625=DIRECTION('center_axis',(1.,0.,0.));
#11626=DIRECTION('ref_axis',(0.,0.,-1.));
#11627=DIRECTION('',(1.,0.,0.));
#11628=DIRECTION('center_axis',(0.,1.,0.));
#11629=DIRECTION('ref_axis',(0.,0.,1.));
#11630=DIRECTION('center_axis',(0.,-1.,0.));
#11631=DIRECTION('ref_axis',(1.,0.,0.));
#11632=DIRECTION('center_axis',(0.,-1.,0.));
#11633=DIRECTION('ref_axis',(1.,0.,0.));
#11634=DIRECTION('center_axis',(0.,-1.,0.));
#11635=DIRECTION('ref_axis',(1.,0.,0.));
#11636=DIRECTION('',(0.707106781186547,0.707106781186548,8.65956056235493E-17));
#11637=DIRECTION('center_axis',(0.,-1.,0.));
#11638=DIRECTION('ref_axis',(1.,0.,0.));
#11639=DIRECTION('center_axis',(0.,-1.,0.));
#11640=DIRECTION('ref_axis',(1.,0.,0.));
#11641=DIRECTION('',(0.,1.,0.));
#11642=DIRECTION('center_axis',(0.,-1.,0.));
#11643=DIRECTION('ref_axis',(0.,0.,-1.));
#11644=DIRECTION('center_axis',(0.,-1.,0.));
#11645=DIRECTION('ref_axis',(1.,0.,0.));
#11646=DIRECTION('center_axis',(0.,-1.,0.));
#11647=DIRECTION('ref_axis',(1.,0.,0.));
#11648=DIRECTION('center_axis',(0.,-1.,0.));
#11649=DIRECTION('ref_axis',(1.,0.,0.));
#11650=DIRECTION('',(0.,1.,0.));
#11651=DIRECTION('',(0.,1.,0.));
#11652=DIRECTION('center_axis',(0.,1.,0.));
#11653=DIRECTION('ref_axis',(1.,0.,0.));
#11654=DIRECTION('center_axis',(0.,-1.,0.));
#11655=DIRECTION('ref_axis',(1.,0.,0.));
#11656=DIRECTION('',(-0.707106781186548,0.707106781186547,-8.65956056235494E-17));
#11657=DIRECTION('center_axis',(0.,-1.,0.));
#11658=DIRECTION('ref_axis',(0.,0.,-1.));
#11659=DIRECTION('axis',(0.,0.,1.));
#11660=DIRECTION('refdir',(1.,0.,0.));
#11661=DIRECTION('center_axis',(0.,1.,0.));
#11662=DIRECTION('ref_axis',(1.,0.,0.));
#11663=DIRECTION('center_axis',(0.,-1.,0.));
#11664=DIRECTION('ref_axis',(1.,0.,0.));
#11665=DIRECTION('',(0.,-1.,0.));
#11666=DIRECTION('center_axis',(0.,-1.,0.));
#11667=DIRECTION('ref_axis',(1.,0.,0.));
#11668=DIRECTION('center_axis',(0.,1.,0.));
#11669=DIRECTION('ref_axis',(1.,0.,0.));
#11670=DIRECTION('center_axis',(0.,1.,0.));
#11671=DIRECTION('ref_axis',(1.,0.,0.));
#11672=DIRECTION('',(0.,-1.,0.));
#11673=DIRECTION('center_axis',(0.,1.,0.));
#11674=DIRECTION('ref_axis',(1.,0.,0.));
#11675=DIRECTION('center_axis',(0.,1.,0.));
#11676=DIRECTION('ref_axis',(1.,0.,0.));
#11677=DIRECTION('center_axis',(0.,1.,0.));
#11678=DIRECTION('ref_axis',(1.,0.,0.));
#11679=DIRECTION('axis',(0.,0.,1.));
#11680=DIRECTION('refdir',(1.,0.,0.));
#11681=DIRECTION('center_axis',(-1.,0.,0.));
#11682=DIRECTION('ref_axis',(0.,0.,1.));
#11683=DIRECTION('center_axis',(0.,-1.,1.38777878078145E-16));
#11684=DIRECTION('ref_axis',(0.,-1.38777878078145E-16,-1.));
#11685=DIRECTION('center_axis',(1.,0.,0.));
#11686=DIRECTION('ref_axis',(0.,0.,1.));
#11687=DIRECTION('center_axis',(0.,1.,0.));
#11688=DIRECTION('ref_axis',(1.,0.,0.));
#11689=DIRECTION('center_axis',(0.,-1.,0.));
#11690=DIRECTION('ref_axis',(1.,0.,0.));
#11691=DIRECTION('',(0.,0.,1.));
#11692=DIRECTION('center_axis',(1.,0.,0.));
#11693=DIRECTION('ref_axis',(0.,0.,1.));
#11694=DIRECTION('',(0.,-1.,0.));
#11695=DIRECTION('',(0.,0.,1.));
#11696=DIRECTION('',(0.,-1.,0.));
#11697=DIRECTION('center_axis',(0.,-1.,0.));
#11698=DIRECTION('ref_axis',(1.,0.,0.));
#11699=DIRECTION('center_axis',(0.,-1.,0.));
#11700=DIRECTION('ref_axis',(1.,0.,0.));
#11701=DIRECTION('',(0.,1.,0.));
#11702=DIRECTION('center_axis',(0.,-1.,0.));
#11703=DIRECTION('ref_axis',(1.,0.,0.));
#11704=DIRECTION('center_axis',(0.,1.,0.));
#11705=DIRECTION('ref_axis',(1.,0.,0.));
#11706=DIRECTION('axis',(0.,0.,1.));
#11707=DIRECTION('refdir',(1.,0.,0.));
#11708=DIRECTION('center_axis',(0.,1.,0.));
#11709=DIRECTION('ref_axis',(1.,0.,0.));
#11710=DIRECTION('center_axis',(0.,1.,0.));
#11711=DIRECTION('ref_axis',(1.,0.,0.));
#11712=DIRECTION('',(0.,-1.,0.));
#11713=DIRECTION('center_axis',(0.,1.,0.));
#11714=DIRECTION('ref_axis',(1.,0.,0.));
#11715=DIRECTION('center_axis',(0.,1.,0.));
#11716=DIRECTION('ref_axis',(1.,0.,0.));
#11717=DIRECTION('center_axis',(0.,1.,0.));
#11718=DIRECTION('ref_axis',(1.,0.,0.));
#11719=DIRECTION('center_axis',(0.,1.,0.));
#11720=DIRECTION('ref_axis',(1.,0.,0.));
#11721=DIRECTION('',(0.,-1.,0.));
#11722=DIRECTION('center_axis',(0.,1.,0.));
#11723=DIRECTION('ref_axis',(1.,0.,0.));
#11724=DIRECTION('center_axis',(0.,1.,0.));
#11725=DIRECTION('ref_axis',(1.,0.,0.));
#11726=DIRECTION('center_axis',(0.,1.,0.));
#11727=DIRECTION('ref_axis',(1.,0.,0.));
#11728=DIRECTION('axis',(0.,0.,1.));
#11729=DIRECTION('refdir',(1.,0.,0.));
#11730=DIRECTION('center_axis',(0.,1.,0.));
#11731=DIRECTION('ref_axis',(1.,0.,0.));
#11732=DIRECTION('center_axis',(0.,1.,0.));
#11733=DIRECTION('ref_axis',(1.,0.,0.));
#11734=DIRECTION('',(0.,-1.,0.));
#11735=DIRECTION('center_axis',(0.,1.,0.));
#11736=DIRECTION('ref_axis',(1.,0.,0.));
#11737=DIRECTION('center_axis',(0.,1.,0.));
#11738=DIRECTION('ref_axis',(1.,0.,0.));
#11739=DIRECTION('center_axis',(0.,1.,0.));
#11740=DIRECTION('ref_axis',(1.,0.,0.));
#11741=DIRECTION('center_axis',(0.,1.,0.));
#11742=DIRECTION('ref_axis',(1.,0.,0.));
#11743=DIRECTION('',(0.,-1.,0.));
#11744=DIRECTION('center_axis',(0.,1.,0.));
#11745=DIRECTION('ref_axis',(1.,0.,0.));
#11746=DIRECTION('center_axis',(0.,1.,0.));
#11747=DIRECTION('ref_axis',(1.,0.,0.));
#11748=DIRECTION('center_axis',(0.,1.,0.));
#11749=DIRECTION('ref_axis',(1.,0.,0.));
#11750=DIRECTION('axis',(0.,0.,1.));
#11751=DIRECTION('refdir',(1.,0.,0.));
#11752=DIRECTION('center_axis',(0.,1.,0.));
#11753=DIRECTION('ref_axis',(1.,0.,0.));
#11754=DIRECTION('center_axis',(0.,1.,0.));
#11755=DIRECTION('ref_axis',(1.,0.,0.));
#11756=DIRECTION('',(0.,1.,0.));
#11757=DIRECTION('center_axis',(0.,-1.,0.));
#11758=DIRECTION('ref_axis',(1.,0.,0.));
#11759=DIRECTION('center_axis',(0.,1.,0.));
#11760=DIRECTION('ref_axis',(1.,0.,0.));
#11761=DIRECTION('center_axis',(0.,1.,0.));
#11762=DIRECTION('ref_axis',(1.,0.,0.));
#11763=DIRECTION('',(0.,1.,0.));
#11764=DIRECTION('center_axis',(0.,-1.,0.));
#11765=DIRECTION('ref_axis',(1.,0.,0.));
#11766=DIRECTION('center_axis',(1.,0.,0.));
#11767=DIRECTION('ref_axis',(0.,0.,-1.));
#11768=DIRECTION('center_axis',(1.,0.,0.));
#11769=DIRECTION('ref_axis',(0.,0.,-1.));
#11770=DIRECTION('',(1.,0.,0.));
#11771=DIRECTION('center_axis',(-1.,0.,0.));
#11772=DIRECTION('ref_axis',(0.,0.,-1.));
#11773=DIRECTION('center_axis',(0.,0.,1.));
#11774=DIRECTION('ref_axis',(1.,0.,0.));
#11775=DIRECTION('',(1.,0.,0.));
#11776=DIRECTION('',(0.,-1.,0.));
#11777=DIRECTION('',(-1.,0.,0.));
#11778=DIRECTION('',(0.,1.,0.));
#11779=DIRECTION('center_axis',(-1.,0.,0.));
#11780=DIRECTION('ref_axis',(0.,-1.,0.));
#11781=DIRECTION('',(0.,0.,-1.));
#11782=DIRECTION('',(0.,-1.,0.));
#11783=DIRECTION('',(0.,0.,1.));
#11784=DIRECTION('center_axis',(0.,1.,0.));
#11785=DIRECTION('ref_axis',(-1.,0.,0.));
#11786=DIRECTION('',(-1.,0.,0.));
#11787=DIRECTION('',(0.,0.,1.));
#11788=DIRECTION('center_axis',(1.,0.,0.));
#11789=DIRECTION('ref_axis',(0.,1.,0.));
#11790=DIRECTION('',(0.,0.,1.));
#11791=DIRECTION('',(0.,1.,0.));
#11792=DIRECTION('center_axis',(0.,0.,1.));
#11793=DIRECTION('ref_axis',(1.,0.,0.));
#11794=DIRECTION('',(-1.,0.,0.));
#11795=DIRECTION('center_axis',(0.,1.,0.));
#11796=DIRECTION('ref_axis',(-1.,0.,0.));
#11797=DIRECTION('',(-1.,0.,0.));
#11798=DIRECTION('',(0.,0.,1.));
#11799=DIRECTION('',(-1.,0.,0.));
#11800=DIRECTION('',(0.,0.,1.));
#11801=DIRECTION('center_axis',(1.,0.,0.));
#11802=DIRECTION('ref_axis',(0.,1.,0.));
#11803=DIRECTION('',(0.,1.,0.));
#11804=DIRECTION('',(0.,1.,0.));
#11805=DIRECTION('',(0.,0.,1.));
#11806=DIRECTION('center_axis',(0.,-1.,0.));
#11807=DIRECTION('ref_axis',(1.,0.,0.));
#11808=DIRECTION('',(1.,0.,0.));
#11809=DIRECTION('',(1.,0.,0.));
#11810=DIRECTION('',(0.,0.,1.));
#11811=DIRECTION('center_axis',(-1.,0.,0.));
#11812=DIRECTION('ref_axis',(0.,-1.,0.));
#11813=DIRECTION('',(0.,-1.,0.));
#11814=DIRECTION('',(0.,-1.,0.));
#11815=DIRECTION('center_axis',(0.,0.,1.));
#11816=DIRECTION('ref_axis',(1.,0.,0.));
#11817=DIRECTION('center_axis',(0.,0.,1.));
#11818=DIRECTION('ref_axis',(1.,0.,0.));
#11819=DIRECTION('axis',(0.,0.,1.));
#11820=DIRECTION('refdir',(1.,0.,0.));
#11821=DIRECTION('center_axis',(0.,1.,0.));
#11822=DIRECTION('ref_axis',(1.,0.,0.));
#11823=DIRECTION('center_axis',(0.,-1.,0.));
#11824=DIRECTION('ref_axis',(1.,0.,0.));
#11825=DIRECTION('',(0.,-1.,0.));
#11826=DIRECTION('center_axis',(0.,-1.,0.));
#11827=DIRECTION('ref_axis',(1.,0.,0.));
#11828=DIRECTION('center_axis',(0.,1.,0.));
#11829=DIRECTION('ref_axis',(1.,0.,0.));
#11830=DIRECTION('center_axis',(0.,1.,0.));
#11831=DIRECTION('ref_axis',(1.,0.,0.));
#11832=DIRECTION('',(0.,-1.,0.));
#11833=DIRECTION('center_axis',(0.,1.,0.));
#11834=DIRECTION('ref_axis',(1.,0.,0.));
#11835=DIRECTION('center_axis',(0.,1.,0.));
#11836=DIRECTION('ref_axis',(1.,0.,0.));
#11837=DIRECTION('center_axis',(0.,1.,0.));
#11838=DIRECTION('ref_axis',(1.,0.,0.));
#11839=DIRECTION('axis',(0.,0.,1.));
#11840=DIRECTION('refdir',(1.,0.,0.));
#11841=DIRECTION('center_axis',(0.,1.,0.));
#11842=DIRECTION('ref_axis',(1.,0.,0.));
#11843=DIRECTION('',(0.866025403784439,-0.5,1.06057523872491E-16));
#11844=DIRECTION('center_axis',(0.,-1.,0.));
#11845=DIRECTION('ref_axis',(1.,0.,0.));
#11846=DIRECTION('center_axis',(0.,-1.,0.));
#11847=DIRECTION('ref_axis',(1.,0.,0.));
#11848=DIRECTION('center_axis',(0.,1.,0.));
#11849=DIRECTION('ref_axis',(1.,0.,0.));
#11850=DIRECTION('',(-0.866025403784439,-0.5,-1.06057523872491E-16));
#11851=DIRECTION('center_axis',(1.92296268638356E-16,0.,-1.));
#11852=DIRECTION('ref_axis',(-1.,0.,-1.92296268638356E-16));
#11853=DIRECTION('',(0.,1.,0.));
#11854=DIRECTION('',(0.,1.,0.));
#11855=DIRECTION('center_axis',(-0.866025403784439,0.,-0.5));
#11856=DIRECTION('ref_axis',(-0.5,0.,0.866025403784439));
#11857=DIRECTION('',(0.,1.,0.));
#11858=DIRECTION('center_axis',(-0.866025403784439,0.,0.5));
#11859=DIRECTION('ref_axis',(0.5,0.,0.866025403784439));
#11860=DIRECTION('',(0.,1.,0.));
#11861=DIRECTION('center_axis',(0.,1.,0.));
#11862=DIRECTION('ref_axis',(1.,0.,0.));
#11863=DIRECTION('center_axis',(0.,1.,0.));
#11864=DIRECTION('ref_axis',(1.,0.,0.));
#11865=DIRECTION('',(0.,-1.,0.));
#11866=DIRECTION('center_axis',(0.,1.,0.));
#11867=DIRECTION('ref_axis',(1.,0.,0.));
#11868=DIRECTION('center_axis',(-1.92296268638356E-16,0.,1.));
#11869=DIRECTION('ref_axis',(1.,0.,1.92296268638356E-16));
#11870=DIRECTION('',(0.,1.,0.));
#11871=DIRECTION('center_axis',(0.866025403784439,0.,-0.5));
#11872=DIRECTION('ref_axis',(-0.5,0.,-0.866025403784439));
#11873=DIRECTION('',(0.,1.,0.));
#11874=DIRECTION('center_axis',(0.866025403784439,0.,0.5));
#11875=DIRECTION('ref_axis',(0.5,0.,-0.866025403784439));
#11876=DIRECTION('center_axis',(0.,1.,0.));
#11877=DIRECTION('ref_axis',(1.,0.,0.));
#11878=DIRECTION('center_axis',(0.,1.,0.));
#11879=DIRECTION('ref_axis',(1.,0.,0.));
#11880=DIRECTION('',(0.,0.,1.));
#11881=DIRECTION('',(1.,0.,0.));
#11882=DIRECTION('',(0.,0.,1.));
#11883=DIRECTION('',(1.,0.,0.));
#11884=DIRECTION('',(0.,0.,1.));
#11885=DIRECTION('',(1.,0.,0.));
#11886=DIRECTION('',(0.,0.,1.));
#11887=DIRECTION('',(1.,0.,0.));
#11888=DIRECTION('',(0.,0.,1.));
#11889=DIRECTION('',(1.,0.,0.));
#11890=DIRECTION('',(0.,-1.,2.22044604925031E-16));
#11891=DIRECTION('',(1.,0.,0.));
#11892=DIRECTION('',(0.,0.,1.));
#11893=DIRECTION('',(2.22044604925031E-16,1.,0.));
#11894=DIRECTION('',(0.,0.,1.));
#11895=DIRECTION('',(2.22044604925031E-16,-1.,0.));
#11896=DIRECTION('',(0.,0.,1.));
#11897=DIRECTION('',(2.22044604925031E-16,-1.,0.));
#11898=DIRECTION('',(0.,0.,1.));
#11899=DIRECTION('',(2.22044604925031E-16,-1.,0.));
#11900=DIRECTION('',(0.,0.,1.));
#11901=DIRECTION('',(1.,0.,0.));
#11902=DIRECTION('',(0.,0.,1.));
#11903=DIRECTION('',(1.,0.,0.));
#11904=DIRECTION('',(0.,0.,1.));
#11905=DIRECTION('',(1.,0.,0.));
#11906=DIRECTION('',(0.,0.,1.));
#11907=DIRECTION('',(1.,0.,0.));
#11908=DIRECTION('',(0.,0.,1.));
#11909=DIRECTION('',(1.,0.,0.));
#11910=DIRECTION('',(0.,0.,1.));
#11911=DIRECTION('',(1.,0.,0.));
#11912=DIRECTION('',(0.,0.,1.));
#11913=DIRECTION('',(1.,0.,0.));
#11914=DIRECTION('',(0.,0.,1.));
#11915=DIRECTION('',(1.,0.,0.));
#11916=DIRECTION('',(0.,0.,1.));
#11917=DIRECTION('',(1.,0.,0.));
#11918=DIRECTION('',(0.,0.,1.));
#11919=DIRECTION('',(1.,0.,0.));
#11920=CARTESIAN_POINT('',(0.,0.,0.));
#11921=CARTESIAN_POINT('',(0.,0.,0.));
#11922=CARTESIAN_POINT('',(0.,0.,0.));
#11923=CARTESIAN_POINT('Origin',(-1.2,0.6,1.9));
#11924=CARTESIAN_POINT('',(-1.41,0.6,2.));
#11925=CARTESIAN_POINT('Origin',(-1.2,0.6,2.));
#11926=CARTESIAN_POINT('',(-1.41,0.6,3.1));
#11927=CARTESIAN_POINT('',(-1.41,0.6,1.9));
#11928=CARTESIAN_POINT('Origin',(-1.2,0.6,3.1));
#11929=CARTESIAN_POINT('Origin',(-1.2,0.6,3.1));
#11930=CARTESIAN_POINT('Origin',(1.2,0.6,1.9));
#11931=CARTESIAN_POINT('',(0.99,0.6,2.));
#11932=CARTESIAN_POINT('Origin',(1.2,0.6,2.));
#11933=CARTESIAN_POINT('',(0.99,0.6,3.1));
#11934=CARTESIAN_POINT('',(0.99,0.6,1.9));
#11935=CARTESIAN_POINT('Origin',(1.2,0.6,3.1));
#11936=CARTESIAN_POINT('Origin',(1.2,0.6,3.1));
#11937=CARTESIAN_POINT('Origin',(0.,0.7,5.4));
#11938=CARTESIAN_POINT('',(0.173205080756888,0.7,5.3));
#11939=CARTESIAN_POINT('',(-0.173205080756888,0.7,5.3));
#11940=CARTESIAN_POINT('',(0.,0.7,5.3));
#11941=CARTESIAN_POINT('Origin',(0.,0.7,5.4));
#11942=CARTESIAN_POINT('Origin',(0.,0.7,5.4));
#11943=CARTESIAN_POINT('',(0.173205080756888,0.7,5.5));
#11944=CARTESIAN_POINT('',(0.173205080756888,0.7,5.3));
#11945=CARTESIAN_POINT('Origin',(0.,0.7,5.4));
#11946=CARTESIAN_POINT('Origin',(0.,0.7,5.4));
#11947=CARTESIAN_POINT('',(0.2,0.8,5.4));
#11948=CARTESIAN_POINT('Origin',(0.,0.8,5.4));
#11949=CARTESIAN_POINT('Origin',(0.,0.8,5.4));
#11950=CARTESIAN_POINT('Origin',(0.,0.7,5.4));
#11951=CARTESIAN_POINT('',(-0.173205080756888,0.9,5.3));
#11952=CARTESIAN_POINT('',(-0.173205080756888,0.7,5.3));
#11953=CARTESIAN_POINT('',(0.173205080756888,0.9,5.3));
#11954=CARTESIAN_POINT('',(0.173205080756888,0.7,5.3));
#11955=CARTESIAN_POINT('Origin',(0.,0.8,5.4));
#11956=CARTESIAN_POINT('',(-0.2,0.8,5.4));
#11957=CARTESIAN_POINT('Origin',(0.,0.8,5.4));
#11958=CARTESIAN_POINT('',(-0.2,1.2,5.4));
#11959=CARTESIAN_POINT('',(-0.2,0.7,5.4));
#11960=CARTESIAN_POINT('',(-0.181811868577262,1.2,5.48333333333333));
#11961=CARTESIAN_POINT('Origin',(0.,1.2,5.4));
#11962=CARTESIAN_POINT('',(-0.181811868577262,1.5,5.48333333333333));
#11963=CARTESIAN_POINT('',(-0.181811868577262,0.7,5.48333333333333));
#11964=CARTESIAN_POINT('',(0.181811868577262,1.5,5.48333333333333));
#11965=CARTESIAN_POINT('Origin',(0.,1.5,5.4));
#11966=CARTESIAN_POINT('',(0.181811868577262,1.2,5.48333333333333));
#11967=CARTESIAN_POINT('',(0.181811868577262,0.7,5.48333333333333));
#11968=CARTESIAN_POINT('Origin',(0.,1.2,5.4));
#11969=CARTESIAN_POINT('Origin',(0.,0.8,5.4));
#11970=CARTESIAN_POINT('Origin',(0.,0.7,5.4));
#11971=CARTESIAN_POINT('',(-0.173205080756888,0.7,5.5));
#11972=CARTESIAN_POINT('Origin',(0.,0.8,5.4));
#11973=CARTESIAN_POINT('Origin',(0.,0.7,5.4));
#11974=CARTESIAN_POINT('Origin',(0.,0.8,5.4));
#11975=CARTESIAN_POINT('Origin',(0.,1.5,5.4));
#11976=CARTESIAN_POINT('Origin',(0.,1.5,4.5));
#11977=CARTESIAN_POINT('Origin',(0.,0.7,5.4));
#11978=CARTESIAN_POINT('',(-0.173205080756888,0.7,5.3));
#11979=CARTESIAN_POINT('Origin',(0.,0.8,5.3));
#11980=CARTESIAN_POINT('Origin',(0.,0.8,5.3));
#11981=CARTESIAN_POINT('Origin',(0.,0.8,5.3));
#11982=CARTESIAN_POINT('Origin',(0.,0.8,5.3));
#11983=CARTESIAN_POINT('Origin',(0.,0.8,5.3));
#11984=CARTESIAN_POINT('Origin',(0.,0.8,5.3));
#11985=CARTESIAN_POINT('',(-0.2,0.8,5.8));
#11986=CARTESIAN_POINT('',(-0.2,0.8,5.3));
#11987=CARTESIAN_POINT('Origin',(0.,0.8,5.8));
#11988=CARTESIAN_POINT('Origin',(0.,0.8,5.3));
#11989=CARTESIAN_POINT('Origin',(0.,0.8,5.3));
#11990=CARTESIAN_POINT('Origin',(0.,1.2,4.5));
#11991=CARTESIAN_POINT('',(-1.,1.2,4.5));
#11992=CARTESIAN_POINT('Origin',(0.,1.2,4.5));
#11993=CARTESIAN_POINT('',(-1.,1.7,4.5));
#11994=CARTESIAN_POINT('',(-1.,1.2,4.5));
#11995=CARTESIAN_POINT('Origin',(0.,1.7,4.5));
#11996=CARTESIAN_POINT('Origin',(0.,1.2,4.5));
#11997=CARTESIAN_POINT('Origin',(0.,0.8,5.3));
#11998=CARTESIAN_POINT('Origin',(0.,0.8,5.8));
#11999=CARTESIAN_POINT('',(-0.685,0.8,5.8));
#12000=CARTESIAN_POINT('Origin',(0.,0.8,5.8));
#12001=CARTESIAN_POINT('',(-0.685,0.8,7.));
#12002=CARTESIAN_POINT('',(-0.685,0.8,5.8));
#12003=CARTESIAN_POINT('Origin',(0.,0.8,7.));
#12004=CARTESIAN_POINT('Origin',(0.,0.8,5.8));
#12005=CARTESIAN_POINT('Origin',(2.,-0.1,2.5));
#12006=CARTESIAN_POINT('',(1.725,0.,2.5));
#12007=CARTESIAN_POINT('Origin',(2.,0.,2.5));
#12008=CARTESIAN_POINT('',(1.725,1.7,2.5));
#12009=CARTESIAN_POINT('',(1.725,-0.1,2.5));
#12010=CARTESIAN_POINT('Origin',(2.,1.7,2.5));
#12011=CARTESIAN_POINT('Origin',(-2.,-0.1,6.5));
#12012=CARTESIAN_POINT('',(-2.275,0.,6.5));
#12013=CARTESIAN_POINT('Origin',(-2.,0.,6.5));
#12014=CARTESIAN_POINT('',(-2.275,1.7,6.5));
#12015=CARTESIAN_POINT('',(-2.275,-0.1,6.5));
#12016=CARTESIAN_POINT('Origin',(-2.,1.7,6.5));
#12017=CARTESIAN_POINT('Origin',(-2.,-0.1,2.5));
#12018=CARTESIAN_POINT('',(-2.275,0.,2.5));
#12019=CARTESIAN_POINT('Origin',(-2.,0.,2.5));
#12020=CARTESIAN_POINT('',(-2.275,1.7,2.5));
#12021=CARTESIAN_POINT('',(-2.275,-0.1,2.5));
#12022=CARTESIAN_POINT('Origin',(-2.,1.7,2.5));
#12023=CARTESIAN_POINT('Origin',(2.,-0.1,6.5));
#12024=CARTESIAN_POINT('',(1.725,0.,6.5));
#12025=CARTESIAN_POINT('Origin',(2.,0.,6.5));
#12026=CARTESIAN_POINT('',(1.725,1.7,6.5));
#12027=CARTESIAN_POINT('',(1.725,-0.1,6.5));
#12028=CARTESIAN_POINT('Origin',(2.,1.7,6.5));
#12029=CARTESIAN_POINT('Origin',(0.,-0.1,4.5));
#12030=CARTESIAN_POINT('',(-0.6,0.,4.5));
#12031=CARTESIAN_POINT('Origin',(0.,0.,4.5));
#12032=CARTESIAN_POINT('',(-0.6,1.2,4.5));
#12033=CARTESIAN_POINT('',(-0.6,-0.1,4.5));
#12034=CARTESIAN_POINT('Origin',(0.,1.2,4.5));
#12035=CARTESIAN_POINT('Origin',(0.,1.2,4.5));
#12036=CARTESIAN_POINT('Origin',(2.5,1.7,2.));
#12037=CARTESIAN_POINT('',(2.5,1.7,2.));
#12038=CARTESIAN_POINT('',(-2.5,1.7,2.));
#12039=CARTESIAN_POINT('',(2.5,1.7,2.));
#12040=CARTESIAN_POINT('',(-2.5,1.7,7.));
#12041=CARTESIAN_POINT('',(-2.5,1.7,2.));
#12042=CARTESIAN_POINT('',(2.5,1.7,7.));
#12043=CARTESIAN_POINT('',(2.5,1.7,7.));
#12044=CARTESIAN_POINT('',(2.5,1.7,2.));
#12045=CARTESIAN_POINT('Origin',(2.5,0.,2.));
#12046=CARTESIAN_POINT('',(2.5,0.,2.));
#12047=CARTESIAN_POINT('',(2.5,0.,2.));
#12048=CARTESIAN_POINT('',(2.5,0.,7.));
#12049=CARTESIAN_POINT('',(2.5,0.,7.));
#12050=CARTESIAN_POINT('',(2.5,0.,2.));
#12051=CARTESIAN_POINT('Origin',(-2.5,0.,2.));
#12052=CARTESIAN_POINT('',(-2.5,0.,2.));
#12053=CARTESIAN_POINT('',(-2.5,0.,2.));
#12054=CARTESIAN_POINT('',(-2.5,0.,7.));
#12055=CARTESIAN_POINT('',(-2.5,0.,7.));
#12056=CARTESIAN_POINT('',(-2.5,0.,2.));
#12057=CARTESIAN_POINT('Origin',(-2.5,1.7,2.));
#12058=CARTESIAN_POINT('',(-2.5,1.7,2.));
#12059=CARTESIAN_POINT('',(-2.5,1.7,7.));
#12060=CARTESIAN_POINT('Origin',(0.,0.85,7.));
#12061=CARTESIAN_POINT('Origin',(0.,0.85,2.));
#12062=CARTESIAN_POINT('',(0.,0.,0.));
#12063=CARTESIAN_POINT('Origin',(0.35,0.8,8.5));
#12064=CARTESIAN_POINT('',(0.35,0.8,9.015));
#12065=CARTESIAN_POINT('Origin',(0.35,0.8,8.5));
#12066=CARTESIAN_POINT('',(1.,0.8,9.015));
#12067=CARTESIAN_POINT('',(0.35,0.8,9.015));
#12068=CARTESIAN_POINT('Origin',(1.,0.8,8.5));
#12069=CARTESIAN_POINT('Origin',(0.35,0.8,8.5));
#12070=CARTESIAN_POINT('',(0.35,0.606350832689629,8.9));
#12071=CARTESIAN_POINT('',(0.35,0.606350832689629,8.2));
#12072=CARTESIAN_POINT('',(0.35,0.606350832689629,8.2));
#12073=CARTESIAN_POINT('',(0.35,0.993649167310371,8.9));
#12074=CARTESIAN_POINT('',(0.35,0.8,8.9));
#12075=CARTESIAN_POINT('',(0.35,0.993649167310371,8.2));
#12076=CARTESIAN_POINT('',(0.35,0.993649167310371,8.2));
#12077=CARTESIAN_POINT('',(0.35,0.8,8.2));
#12078=CARTESIAN_POINT('Origin',(0.,0.8,8.9));
#12079=CARTESIAN_POINT('Origin',(0.,0.8,8.9));
#12080=CARTESIAN_POINT('',(-0.25,0.8,8.9));
#12081=CARTESIAN_POINT('Origin',(0.,0.8,8.9));
#12082=CARTESIAN_POINT('Origin',(0.,0.8,8.2));
#12083=CARTESIAN_POINT('Origin',(0.,0.8,8.2));
#12084=CARTESIAN_POINT('Origin',(0.,0.8,9.2));
#12085=CARTESIAN_POINT('',(-0.49,0.8,9.2));
#12086=CARTESIAN_POINT('Origin',(0.,0.8,9.2));
#12087=CARTESIAN_POINT('',(-0.49,0.8,9.4));
#12088=CARTESIAN_POINT('',(-0.49,0.8,9.2));
#12089=CARTESIAN_POINT('Origin',(0.,0.8,9.4));
#12090=CARTESIAN_POINT('Origin',(0.,0.8,9.4));
#12091=CARTESIAN_POINT('',(-0.25,0.8,9.4));
#12092=CARTESIAN_POINT('Origin',(0.,0.8,9.4));
#12093=CARTESIAN_POINT('Origin',(0.,0.8,9.2));
#12094=CARTESIAN_POINT('',(-0.25,0.8,9.2));
#12095=CARTESIAN_POINT('Origin',(0.,0.8,9.2));
#12096=CARTESIAN_POINT('Origin',(0.,0.8,8.8));
#12097=CARTESIAN_POINT('',(-0.25,0.8,8.8));
#12098=CARTESIAN_POINT('Origin',(0.,0.8,8.8));
#12099=CARTESIAN_POINT('',(-0.25,0.8,9.5));
#12100=CARTESIAN_POINT('',(-0.25,0.8,8.8));
#12101=CARTESIAN_POINT('Origin',(0.,0.8,9.5));
#12102=CARTESIAN_POINT('Origin',(0.,0.8,8.2));
#12103=CARTESIAN_POINT('',(-0.2,0.8,8.2));
#12104=CARTESIAN_POINT('Origin',(0.,0.8,8.2));
#12105=CARTESIAN_POINT('Origin',(0.,0.8,7.5));
#12106=CARTESIAN_POINT('',(-1.,0.782050807568877,7.5));
#12107=CARTESIAN_POINT('',(-0.505181485540923,-0.0749999999999997,7.5));
#12108=CARTESIAN_POINT('',(-1.01036297108185,0.8,7.5));
#12109=CARTESIAN_POINT('',(0.505181485540923,-0.075,7.5));
#12110=CARTESIAN_POINT('',(-0.505181485540923,-0.0749999999999997,7.5));
#12111=CARTESIAN_POINT('',(1.,0.782050807568877,7.5));
#12112=CARTESIAN_POINT('',(0.505181485540923,-0.075,7.5));
#12113=CARTESIAN_POINT('',(1.,-0.2,7.5));
#12114=CARTESIAN_POINT('',(1.,-0.2,7.5));
#12115=CARTESIAN_POINT('',(-1.,-0.2,7.5));
#12116=CARTESIAN_POINT('',(-1.,-0.2,7.5));
#12117=CARTESIAN_POINT('',(-1.,1.8,7.5));
#12118=CARTESIAN_POINT('Origin',(1.,1.8,7.5));
#12119=CARTESIAN_POINT('',(1.,1.8,7.5));
#12120=CARTESIAN_POINT('',(-1.,1.8,7.5));
#12121=CARTESIAN_POINT('',(1.,1.8,7.5));
#12122=CARTESIAN_POINT('',(-1.,1.8,9.5));
#12123=CARTESIAN_POINT('',(-1.,1.8,7.5));
#12124=CARTESIAN_POINT('',(1.,1.8,9.5));
#12125=CARTESIAN_POINT('',(1.,1.8,9.5));
#12126=CARTESIAN_POINT('',(1.,1.8,7.5));
#12127=CARTESIAN_POINT('Origin',(1.,-0.2,7.5));
#12128=CARTESIAN_POINT('',(1.,0.817949192431123,7.5));
#12129=CARTESIAN_POINT('',(1.,0.3,7.5));
#12130=CARTESIAN_POINT('',(1.,-0.2,7.5));
#12131=CARTESIAN_POINT('',(1.,-0.2,9.5));
#12132=CARTESIAN_POINT('',(1.,-0.2,9.5));
#12133=CARTESIAN_POINT('',(1.,-0.2,7.5));
#12134=CARTESIAN_POINT('Origin',(-1.,-0.2,7.5));
#12135=CARTESIAN_POINT('',(-1.,-0.2,9.5));
#12136=CARTESIAN_POINT('',(-1.,-0.2,9.5));
#12137=CARTESIAN_POINT('',(-1.,-0.2,7.5));
#12138=CARTESIAN_POINT('Origin',(-1.,1.8,7.5));
#12139=CARTESIAN_POINT('',(-1.,0.817949192431123,7.5));
#12140=CARTESIAN_POINT('',(-1.,1.8,7.5));
#12141=CARTESIAN_POINT('',(-1.,1.3,7.5));
#12142=CARTESIAN_POINT('',(-1.,1.8,9.5));
#12143=CARTESIAN_POINT('Origin',(0.,0.8,9.5));
#12144=CARTESIAN_POINT('Origin',(0.,0.8,7.5));
#12145=CARTESIAN_POINT('',(-0.505181485540922,1.675,7.5));
#12146=CARTESIAN_POINT('',(-0.505181485540922,1.675,7.5));
#12147=CARTESIAN_POINT('',(0.505181485540923,1.675,7.5));
#12148=CARTESIAN_POINT('',(1.01036297108185,0.8,7.5));
#12149=CARTESIAN_POINT('',(0.505181485540923,1.675,7.5));
#12150=CARTESIAN_POINT('Origin',(0.,0.8,7.5));
#12151=CARTESIAN_POINT('',(1.01036297108185,0.8,7.5));
#12152=CARTESIAN_POINT('',(0.505181485540923,-0.075,7.5));
#12153=CARTESIAN_POINT('',(1.01036297108185,0.8,7.5));
#12154=CARTESIAN_POINT('Origin',(0.,0.8,7.));
#12155=CARTESIAN_POINT('',(0.505181485540923,-0.075,7.));
#12156=CARTESIAN_POINT('',(1.01036297108185,0.8,7.));
#12157=CARTESIAN_POINT('',(0.505181485540923,-0.075,7.));
#12158=CARTESIAN_POINT('',(-0.505181485540923,-0.0749999999999997,7.));
#12159=CARTESIAN_POINT('',(-0.505181485540923,-0.0749999999999997,7.));
#12160=CARTESIAN_POINT('',(-1.01036297108185,0.8,7.));
#12161=CARTESIAN_POINT('',(-1.01036297108185,0.8,7.));
#12162=CARTESIAN_POINT('',(-0.505181485540922,1.675,7.));
#12163=CARTESIAN_POINT('',(-0.505181485540922,1.675,7.));
#12164=CARTESIAN_POINT('',(0.505181485540923,1.675,7.));
#12165=CARTESIAN_POINT('',(0.505181485540923,1.675,7.));
#12166=CARTESIAN_POINT('',(1.01036297108185,0.8,7.));
#12167=CARTESIAN_POINT('',(-0.685,0.8,7.));
#12168=CARTESIAN_POINT('Origin',(0.,0.8,7.));
#12169=CARTESIAN_POINT('Origin',(-0.505181485540923,-0.0749999999999997,
7.));
#12170=CARTESIAN_POINT('',(0.505181485540923,-0.075,7.));
#12171=CARTESIAN_POINT('',(-0.505181485540923,-0.0749999999999997,7.));
#12172=CARTESIAN_POINT('Origin',(-1.01036297108185,0.8,7.));
#12173=CARTESIAN_POINT('',(-1.01036297108185,0.8,7.5));
#12174=CARTESIAN_POINT('',(-1.01036297108185,0.8,7.5));
#12175=CARTESIAN_POINT('',(-1.01036297108185,0.8,7.));
#12176=CARTESIAN_POINT('Origin',(-0.505181485540922,1.675,7.));
#12177=CARTESIAN_POINT('',(-0.505181485540922,1.675,7.5));
#12178=CARTESIAN_POINT('',(-0.505181485540922,1.675,7.));
#12179=CARTESIAN_POINT('Origin',(0.505181485540923,1.675,7.));
#12180=CARTESIAN_POINT('',(0.505181485540923,1.675,7.));
#12181=CARTESIAN_POINT('Origin',(1.01036297108185,0.8,7.));
#12182=CARTESIAN_POINT('',(1.01036297108185,0.8,7.));
#12183=CARTESIAN_POINT('Origin',(0.505181485540923,-0.075,7.));
#12184=CARTESIAN_POINT('Origin',(0.,0.8,7.5));
#12185=CARTESIAN_POINT('Origin',(0.,0.8,5.8));
#12186=CARTESIAN_POINT('',(-0.2,0.8,5.8));
#12187=CARTESIAN_POINT('',(-0.2,0.8,5.8));
#12188=CARTESIAN_POINT('Origin',(0.,0.8,5.8));
#12189=CARTESIAN_POINT('Origin',(0.,0.8,5.8));
#12190=CARTESIAN_POINT('',(-0.685,0.8,5.8));
#12191=CARTESIAN_POINT('',(-0.685,0.8,5.8));
#12192=CARTESIAN_POINT('Origin',(0.,0.8,5.8));
#12193=CARTESIAN_POINT('Origin',(0.,0.8,5.8));
#12194=CARTESIAN_POINT('',(0.,0.,0.));
#12195=CARTESIAN_POINT('Origin',(0.,0.8,8.15));
#12196=CARTESIAN_POINT('',(-0.2,0.8,8.25));
#12197=CARTESIAN_POINT('Origin',(0.,0.8,8.25));
#12198=CARTESIAN_POINT('',(0.,0.8,8.05));
#12199=CARTESIAN_POINT('',(-0.1,0.8,8.15));
#12200=CARTESIAN_POINT('Origin',(0.,0.8,8.4));
#12201=CARTESIAN_POINT('',(-0.3,0.8,8.55));
#12202=CARTESIAN_POINT('Origin',(0.,0.8,8.55));
#12203=CARTESIAN_POINT('',(-0.25,0.8,8.4));
#12204=CARTESIAN_POINT('Origin',(0.,0.8,9.425));
#12205=CARTESIAN_POINT('',(-0.3,0.8,10.3));
#12206=CARTESIAN_POINT('Origin',(0.,0.8,10.3));
#12207=CARTESIAN_POINT('',(-0.3,0.8,9.425));
#12208=CARTESIAN_POINT('Origin',(0.6,0.8,10.3));
#12209=CARTESIAN_POINT('',(-0.6,0.8,10.3));
#12210=CARTESIAN_POINT('Origin',(0.,0.8,10.3));
#12211=CARTESIAN_POINT('Origin',(0.,0.8,10.6));
#12212=CARTESIAN_POINT('',(-0.6,0.8,10.9));
#12213=CARTESIAN_POINT('Origin',(0.,0.8,10.9));
#12214=CARTESIAN_POINT('',(-0.6,0.8,10.6));
#12215=CARTESIAN_POINT('Origin',(0.,0.8,10.9));
#12216=CARTESIAN_POINT('',(0.,0.,0.));
#12217=CARTESIAN_POINT('Origin',(-1.2,12.,1.9));
#12218=CARTESIAN_POINT('',(-1.41,12.,2.));
#12219=CARTESIAN_POINT('Origin',(-1.2,12.,2.));
#12220=CARTESIAN_POINT('',(-1.41,12.,3.1));
#12221=CARTESIAN_POINT('',(-1.41,12.,1.9));
#12222=CARTESIAN_POINT('Origin',(-1.2,12.,3.1));
#12223=CARTESIAN_POINT('Origin',(-1.2,12.,3.1));
#12224=CARTESIAN_POINT('Origin',(1.2,12.,1.9));
#12225=CARTESIAN_POINT('',(0.99,12.,2.));
#12226=CARTESIAN_POINT('Origin',(1.2,12.,2.));
#12227=CARTESIAN_POINT('',(0.99,12.,3.1));
#12228=CARTESIAN_POINT('',(0.99,12.,1.9));
#12229=CARTESIAN_POINT('Origin',(1.2,12.,3.1));
#12230=CARTESIAN_POINT('Origin',(1.2,12.,3.1));
#12231=CARTESIAN_POINT('Origin',(0.,11.9,5.4));
#12232=CARTESIAN_POINT('',(-0.173205080756887,11.9,5.3));
#12233=CARTESIAN_POINT('',(0.173205080756887,11.9,5.3));
#12234=CARTESIAN_POINT('',(0.,11.9,5.3));
#12235=CARTESIAN_POINT('Origin',(0.,11.9,5.4));
#12236=CARTESIAN_POINT('Origin',(0.,11.9,5.4));
#12237=CARTESIAN_POINT('',(0.173205080756887,11.9,5.5));
#12238=CARTESIAN_POINT('',(0.173205080756887,11.9,5.3));
#12239=CARTESIAN_POINT('Origin',(0.,11.9,5.4));
#12240=CARTESIAN_POINT('Origin',(0.,11.9,5.4));
#12241=CARTESIAN_POINT('',(-0.173205080756887,11.9,5.5));
#12242=CARTESIAN_POINT('',(-0.173205080756887,11.9,5.3));
#12243=CARTESIAN_POINT('Origin',(0.,11.9,5.4));
#12244=CARTESIAN_POINT('Origin',(0.,11.1,5.4));
#12245=CARTESIAN_POINT('',(0.181811868577262,11.1,5.48333333333333));
#12246=CARTESIAN_POINT('',(0.181811868577262,11.4,5.48333333333333));
#12247=CARTESIAN_POINT('',(0.181811868577262,11.1,5.48333333333333));
#12248=CARTESIAN_POINT('',(-0.181811868577262,11.1,5.48333333333333));
#12249=CARTESIAN_POINT('Origin',(0.,11.1,5.4));
#12250=CARTESIAN_POINT('',(-0.181811868577262,11.4,5.48333333333333));
#12251=CARTESIAN_POINT('',(-0.181811868577262,11.1,5.48333333333333));
#12252=CARTESIAN_POINT('',(-0.2,11.4,5.4));
#12253=CARTESIAN_POINT('Origin',(0.,11.4,5.4));
#12254=CARTESIAN_POINT('',(-0.2,11.8,5.4));
#12255=CARTESIAN_POINT('',(-0.2,11.1,5.4));
#12256=CARTESIAN_POINT('',(0.2,11.8,5.4));
#12257=CARTESIAN_POINT('Origin',(0.,11.8,5.4));
#12258=CARTESIAN_POINT('',(0.173205080756888,11.7,5.3));
#12259=CARTESIAN_POINT('Origin',(0.,11.8,5.4));
#12260=CARTESIAN_POINT('',(0.173205080756888,11.1,5.3));
#12261=CARTESIAN_POINT('',(-0.173205080756888,11.7,5.3));
#12262=CARTESIAN_POINT('',(-0.173205080756888,11.1,5.3));
#12263=CARTESIAN_POINT('Origin',(0.,11.8,5.4));
#12264=CARTESIAN_POINT('Origin',(0.,11.4,5.4));
#12265=CARTESIAN_POINT('Origin',(0.,11.1,5.4));
#12266=CARTESIAN_POINT('Origin',(0.,11.8,5.4));
#12267=CARTESIAN_POINT('Origin',(0.,11.8,5.4));
#12268=CARTESIAN_POINT('Origin',(0.,11.1,5.4));
#12269=CARTESIAN_POINT('Origin',(0.,11.8,5.4));
#12270=CARTESIAN_POINT('Origin',(0.,11.8,5.4));
#12271=CARTESIAN_POINT('Origin',(0.,11.1,5.4));
#12272=CARTESIAN_POINT('Origin',(0.,11.1,4.5));
#12273=CARTESIAN_POINT('Origin',(0.,11.8,5.3));
#12274=CARTESIAN_POINT('Origin',(0.,11.8,5.3));
#12275=CARTESIAN_POINT('Origin',(0.,11.8,5.3));
#12276=CARTESIAN_POINT('Origin',(0.,11.8,5.3));
#12277=CARTESIAN_POINT('Origin',(0.,11.8,5.3));
#12278=CARTESIAN_POINT('Origin',(0.,11.8,5.3));
#12279=CARTESIAN_POINT('Origin',(0.,11.8,5.3));
#12280=CARTESIAN_POINT('Origin',(0.,11.8,5.3));
#12281=CARTESIAN_POINT('Origin',(0.,11.8,5.3));
#12282=CARTESIAN_POINT('',(-0.2,11.8,5.8));
#12283=CARTESIAN_POINT('',(-0.2,11.8,5.3));
#12284=CARTESIAN_POINT('Origin',(0.,11.8,5.8));
#12285=CARTESIAN_POINT('Origin',(0.,11.4,4.5));
#12286=CARTESIAN_POINT('',(-1.,11.4,4.5));
#12287=CARTESIAN_POINT('Origin',(0.,11.4,4.5));
#12288=CARTESIAN_POINT('Origin',(0.,11.4,4.5));
#12289=CARTESIAN_POINT('Origin',(0.,11.8,5.8));
#12290=CARTESIAN_POINT('',(-0.685,11.8,5.8));
#12291=CARTESIAN_POINT('Origin',(0.,11.8,5.8));
#12292=CARTESIAN_POINT('',(-0.685,11.8,7.));
#12293=CARTESIAN_POINT('',(-0.685,11.8,5.8));
#12294=CARTESIAN_POINT('Origin',(0.,11.8,7.));
#12295=CARTESIAN_POINT('Origin',(0.,11.8,5.8));
#12296=CARTESIAN_POINT('Origin',(2.,10.8,2.5));
#12297=CARTESIAN_POINT('',(1.725,10.9,2.5));
#12298=CARTESIAN_POINT('Origin',(2.,10.9,2.5));
#12299=CARTESIAN_POINT('',(1.725,12.6,2.5));
#12300=CARTESIAN_POINT('',(1.725,10.8,2.5));
#12301=CARTESIAN_POINT('Origin',(2.,12.6,2.5));
#12302=CARTESIAN_POINT('Origin',(-2.,10.8,6.5));
#12303=CARTESIAN_POINT('',(-2.275,10.9,6.5));
#12304=CARTESIAN_POINT('Origin',(-2.,10.9,6.5));
#12305=CARTESIAN_POINT('',(-2.275,12.6,6.5));
#12306=CARTESIAN_POINT('',(-2.275,10.8,6.5));
#12307=CARTESIAN_POINT('Origin',(-2.,12.6,6.5));
#12308=CARTESIAN_POINT('Origin',(-2.,10.8,2.5));
#12309=CARTESIAN_POINT('',(-2.275,10.9,2.5));
#12310=CARTESIAN_POINT('Origin',(-2.,10.9,2.5));
#12311=CARTESIAN_POINT('',(-2.275,12.6,2.5));
#12312=CARTESIAN_POINT('',(-2.275,10.8,2.5));
#12313=CARTESIAN_POINT('Origin',(-2.,12.6,2.5));
#12314=CARTESIAN_POINT('Origin',(2.,10.8,6.5));
#12315=CARTESIAN_POINT('',(1.725,10.9,6.5));
#12316=CARTESIAN_POINT('Origin',(2.,10.9,6.5));
#12317=CARTESIAN_POINT('',(1.725,12.6,6.5));
#12318=CARTESIAN_POINT('',(1.725,10.8,6.5));
#12319=CARTESIAN_POINT('Origin',(2.,12.6,6.5));
#12320=CARTESIAN_POINT('Origin',(0.,10.8,4.5));
#12321=CARTESIAN_POINT('',(-1.,10.9,4.5));
#12322=CARTESIAN_POINT('Origin',(0.,10.9,4.5));
#12323=CARTESIAN_POINT('',(-1.,10.8,4.5));
#12324=CARTESIAN_POINT('Origin',(2.5,12.6,2.));
#12325=CARTESIAN_POINT('',(2.5,12.6,2.));
#12326=CARTESIAN_POINT('',(-2.5,12.6,2.));
#12327=CARTESIAN_POINT('',(2.5,12.6,2.));
#12328=CARTESIAN_POINT('',(-2.5,12.6,7.));
#12329=CARTESIAN_POINT('',(-2.5,12.6,2.));
#12330=CARTESIAN_POINT('',(2.5,12.6,7.));
#12331=CARTESIAN_POINT('',(2.5,12.6,7.));
#12332=CARTESIAN_POINT('',(2.5,12.6,2.));
#12333=CARTESIAN_POINT('Origin',(2.5,10.9,2.));
#12334=CARTESIAN_POINT('',(2.5,10.9,2.));
#12335=CARTESIAN_POINT('',(2.5,10.9,2.));
#12336=CARTESIAN_POINT('',(2.5,10.9,7.));
#12337=CARTESIAN_POINT('',(2.5,10.9,7.));
#12338=CARTESIAN_POINT('',(2.5,10.9,2.));
#12339=CARTESIAN_POINT('Origin',(-2.5,10.9,2.));
#12340=CARTESIAN_POINT('',(-2.5,10.9,2.));
#12341=CARTESIAN_POINT('',(-2.5,10.9,2.));
#12342=CARTESIAN_POINT('',(-2.5,10.9,7.));
#12343=CARTESIAN_POINT('',(-2.5,10.9,7.));
#12344=CARTESIAN_POINT('',(-2.5,10.9,2.));
#12345=CARTESIAN_POINT('Origin',(-2.5,12.6,2.));
#12346=CARTESIAN_POINT('',(-2.5,12.6,2.));
#12347=CARTESIAN_POINT('',(-2.5,12.6,7.));
#12348=CARTESIAN_POINT('Origin',(0.,11.75,7.));
#12349=CARTESIAN_POINT('Origin',(0.,11.75,2.));
#12350=CARTESIAN_POINT('',(0.,0.,0.));
#12351=CARTESIAN_POINT('Origin',(0.35,11.8,8.5));
#12352=CARTESIAN_POINT('',(0.35,11.8,9.015));
#12353=CARTESIAN_POINT('Origin',(0.35,11.8,8.5));
#12354=CARTESIAN_POINT('',(1.,11.8,9.015));
#12355=CARTESIAN_POINT('',(0.35,11.8,9.015));
#12356=CARTESIAN_POINT('Origin',(1.,11.8,8.5));
#12357=CARTESIAN_POINT('Origin',(0.35,11.8,8.5));
#12358=CARTESIAN_POINT('',(0.35,11.6063508326896,8.9));
#12359=CARTESIAN_POINT('',(0.35,11.6063508326896,8.2));
#12360=CARTESIAN_POINT('',(0.35,11.6063508326896,8.2));
#12361=CARTESIAN_POINT('',(0.35,11.9936491673104,8.9));
#12362=CARTESIAN_POINT('',(0.35,11.8,8.9));
#12363=CARTESIAN_POINT('',(0.35,11.9936491673104,8.2));
#12364=CARTESIAN_POINT('',(0.35,11.9936491673104,8.2));
#12365=CARTESIAN_POINT('',(0.35,11.8,8.2));
#12366=CARTESIAN_POINT('Origin',(0.,11.8,8.9));
#12367=CARTESIAN_POINT('Origin',(0.,11.8,8.9));
#12368=CARTESIAN_POINT('',(-0.25,11.8,8.9));
#12369=CARTESIAN_POINT('Origin',(0.,11.8,8.9));
#12370=CARTESIAN_POINT('Origin',(0.,11.8,8.2));
#12371=CARTESIAN_POINT('Origin',(0.,11.8,8.2));
#12372=CARTESIAN_POINT('Origin',(0.,11.8,9.2));
#12373=CARTESIAN_POINT('',(-0.49,11.8,9.2));
#12374=CARTESIAN_POINT('Origin',(0.,11.8,9.2));
#12375=CARTESIAN_POINT('',(-0.49,11.8,9.4));
#12376=CARTESIAN_POINT('',(-0.49,11.8,9.2));
#12377=CARTESIAN_POINT('Origin',(0.,11.8,9.4));
#12378=CARTESIAN_POINT('Origin',(0.,11.8,9.4));
#12379=CARTESIAN_POINT('',(-0.25,11.8,9.4));
#12380=CARTESIAN_POINT('Origin',(0.,11.8,9.4));
#12381=CARTESIAN_POINT('Origin',(0.,11.8,9.2));
#12382=CARTESIAN_POINT('',(-0.25,11.8,9.2));
#12383=CARTESIAN_POINT('Origin',(0.,11.8,9.2));
#12384=CARTESIAN_POINT('Origin',(0.,11.8,8.8));
#12385=CARTESIAN_POINT('',(-0.25,11.8,8.8));
#12386=CARTESIAN_POINT('Origin',(0.,11.8,8.8));
#12387=CARTESIAN_POINT('',(-0.25,11.8,9.5));
#12388=CARTESIAN_POINT('',(-0.25,11.8,8.8));
#12389=CARTESIAN_POINT('Origin',(0.,11.8,9.5));
#12390=CARTESIAN_POINT('Origin',(0.,11.8,8.2));
#12391=CARTESIAN_POINT('',(-0.2,11.8,8.2));
#12392=CARTESIAN_POINT('Origin',(0.,11.8,8.2));
#12393=CARTESIAN_POINT('Origin',(0.,11.8,7.5));
#12394=CARTESIAN_POINT('',(-1.,11.7820508075689,7.5));
#12395=CARTESIAN_POINT('',(-0.505181485540923,10.925,7.5));
#12396=CARTESIAN_POINT('',(-1.01036297108185,11.8,7.5));
#12397=CARTESIAN_POINT('',(0.505181485540923,10.925,7.5));
#12398=CARTESIAN_POINT('',(-0.505181485540923,10.925,7.5));
#12399=CARTESIAN_POINT('',(1.,11.7820508075689,7.5));
#12400=CARTESIAN_POINT('',(0.505181485540923,10.925,7.5));
#12401=CARTESIAN_POINT('',(1.,10.8,7.5));
#12402=CARTESIAN_POINT('',(1.,10.8,7.5));
#12403=CARTESIAN_POINT('',(-1.,10.8,7.5));
#12404=CARTESIAN_POINT('',(-1.,10.8,7.5));
#12405=CARTESIAN_POINT('',(-1.,12.8,7.5));
#12406=CARTESIAN_POINT('Origin',(1.,12.8,7.5));
#12407=CARTESIAN_POINT('',(1.,12.8,7.5));
#12408=CARTESIAN_POINT('',(-1.,12.8,7.5));
#12409=CARTESIAN_POINT('',(1.,12.8,7.5));
#12410=CARTESIAN_POINT('',(-1.,12.8,9.5));
#12411=CARTESIAN_POINT('',(-1.,12.8,7.5));
#12412=CARTESIAN_POINT('',(1.,12.8,9.5));
#12413=CARTESIAN_POINT('',(1.,12.8,9.5));
#12414=CARTESIAN_POINT('',(1.,12.8,7.5));
#12415=CARTESIAN_POINT('Origin',(1.,10.8,7.5));
#12416=CARTESIAN_POINT('',(1.,11.8179491924311,7.5));
#12417=CARTESIAN_POINT('',(1.,11.3,7.5));
#12418=CARTESIAN_POINT('',(1.,10.8,7.5));
#12419=CARTESIAN_POINT('',(1.,10.8,9.5));
#12420=CARTESIAN_POINT('',(1.,10.8,9.5));
#12421=CARTESIAN_POINT('',(1.,10.8,7.5));
#12422=CARTESIAN_POINT('Origin',(-1.,10.8,7.5));
#12423=CARTESIAN_POINT('',(-1.,10.8,9.5));
#12424=CARTESIAN_POINT('',(-1.,10.8,9.5));
#12425=CARTESIAN_POINT('',(-1.,10.8,7.5));
#12426=CARTESIAN_POINT('Origin',(-1.,12.8,7.5));
#12427=CARTESIAN_POINT('',(-1.,11.8179491924311,7.5));
#12428=CARTESIAN_POINT('',(-1.,12.8,7.5));
#12429=CARTESIAN_POINT('',(-1.,12.3,7.5));
#12430=CARTESIAN_POINT('',(-1.,12.8,9.5));
#12431=CARTESIAN_POINT('Origin',(0.,11.8,9.5));
#12432=CARTESIAN_POINT('Origin',(0.,11.8,7.5));
#12433=CARTESIAN_POINT('',(-0.505181485540922,12.675,7.5));
#12434=CARTESIAN_POINT('',(-0.505181485540922,12.675,7.5));
#12435=CARTESIAN_POINT('',(0.505181485540923,12.675,7.5));
#12436=CARTESIAN_POINT('',(1.01036297108185,11.8,7.5));
#12437=CARTESIAN_POINT('',(0.505181485540923,12.675,7.5));
#12438=CARTESIAN_POINT('Origin',(0.,11.8,7.5));
#12439=CARTESIAN_POINT('',(1.01036297108185,11.8,7.5));
#12440=CARTESIAN_POINT('',(0.505181485540923,10.925,7.5));
#12441=CARTESIAN_POINT('',(1.01036297108185,11.8,7.5));
#12442=CARTESIAN_POINT('Origin',(0.,11.8,7.));
#12443=CARTESIAN_POINT('',(0.505181485540923,10.925,7.));
#12444=CARTESIAN_POINT('',(1.01036297108185,11.8,7.));
#12445=CARTESIAN_POINT('',(0.505181485540923,10.925,7.));
#12446=CARTESIAN_POINT('',(-0.505181485540923,10.925,7.));
#12447=CARTESIAN_POINT('',(-0.505181485540923,10.925,7.));
#12448=CARTESIAN_POINT('',(-1.01036297108185,11.8,7.));
#12449=CARTESIAN_POINT('',(-1.01036297108185,11.8,7.));
#12450=CARTESIAN_POINT('',(-0.505181485540922,12.675,7.));
#12451=CARTESIAN_POINT('',(-0.505181485540922,12.675,7.));
#12452=CARTESIAN_POINT('',(0.505181485540923,12.675,7.));
#12453=CARTESIAN_POINT('',(0.505181485540923,12.675,7.));
#12454=CARTESIAN_POINT('',(1.01036297108185,11.8,7.));
#12455=CARTESIAN_POINT('',(-0.685,11.8,7.));
#12456=CARTESIAN_POINT('Origin',(0.,11.8,7.));
#12457=CARTESIAN_POINT('Origin',(-0.505181485540923,10.925,7.));
#12458=CARTESIAN_POINT('',(0.505181485540923,10.925,7.));
#12459=CARTESIAN_POINT('',(-0.505181485540923,10.925,7.));
#12460=CARTESIAN_POINT('Origin',(-1.01036297108185,11.8,7.));
#12461=CARTESIAN_POINT('',(-1.01036297108185,11.8,7.5));
#12462=CARTESIAN_POINT('',(-1.01036297108185,11.8,7.5));
#12463=CARTESIAN_POINT('',(-1.01036297108185,11.8,7.));
#12464=CARTESIAN_POINT('Origin',(-0.505181485540922,12.675,7.));
#12465=CARTESIAN_POINT('',(-0.505181485540922,12.675,7.5));
#12466=CARTESIAN_POINT('',(-0.505181485540922,12.675,7.));
#12467=CARTESIAN_POINT('Origin',(0.505181485540923,12.675,7.));
#12468=CARTESIAN_POINT('',(0.505181485540923,12.675,7.));
#12469=CARTESIAN_POINT('Origin',(1.01036297108185,11.8,7.));
#12470=CARTESIAN_POINT('',(1.01036297108185,11.8,7.));
#12471=CARTESIAN_POINT('Origin',(0.505181485540923,10.925,7.));
#12472=CARTESIAN_POINT('Origin',(0.,11.8,7.5));
#12473=CARTESIAN_POINT('Origin',(0.,11.8,5.8));
#12474=CARTESIAN_POINT('',(-0.2,11.8,5.8));
#12475=CARTESIAN_POINT('',(-0.2,11.8,5.8));
#12476=CARTESIAN_POINT('Origin',(0.,11.8,5.8));
#12477=CARTESIAN_POINT('Origin',(0.,11.8,5.8));
#12478=CARTESIAN_POINT('',(-0.685,11.8,5.8));
#12479=CARTESIAN_POINT('',(-0.685,11.8,5.8));
#12480=CARTESIAN_POINT('Origin',(0.,11.8,5.8));
#12481=CARTESIAN_POINT('Origin',(0.,11.8,5.8));
#12482=CARTESIAN_POINT('',(0.,0.,0.));
#12483=CARTESIAN_POINT('Origin',(0.,11.8,8.15));
#12484=CARTESIAN_POINT('',(-0.2,11.8,8.25));
#12485=CARTESIAN_POINT('Origin',(0.,11.8,8.25));
#12486=CARTESIAN_POINT('',(0.,11.8,8.05));
#12487=CARTESIAN_POINT('',(-0.1,11.8,8.15));
#12488=CARTESIAN_POINT('Origin',(0.,11.8,8.4));
#12489=CARTESIAN_POINT('',(-0.3,11.8,8.55));
#12490=CARTESIAN_POINT('Origin',(0.,11.8,8.55));
#12491=CARTESIAN_POINT('',(-0.25,11.8,8.4));
#12492=CARTESIAN_POINT('Origin',(0.,11.8,9.425));
#12493=CARTESIAN_POINT('',(-0.3,11.8,10.3));
#12494=CARTESIAN_POINT('Origin',(0.,11.8,10.3));
#12495=CARTESIAN_POINT('',(-0.3,11.8,9.425));
#12496=CARTESIAN_POINT('Origin',(0.6,11.8,10.3));
#12497=CARTESIAN_POINT('',(-0.6,11.8,10.3));
#12498=CARTESIAN_POINT('Origin',(0.,11.8,10.3));
#12499=CARTESIAN_POINT('Origin',(0.,11.8,10.6));
#12500=CARTESIAN_POINT('',(-0.6,11.8,10.9));
#12501=CARTESIAN_POINT('Origin',(0.,11.8,10.9));
#12502=CARTESIAN_POINT('',(-0.6,11.8,10.6));
#12503=CARTESIAN_POINT('Origin',(0.,11.8,10.9));
#12504=CARTESIAN_POINT('',(0.,0.,0.));
#12505=CARTESIAN_POINT('Origin',(0.,1.8,4.5));
#12506=CARTESIAN_POINT('',(-1.,10.8,4.5));
#12507=CARTESIAN_POINT('Origin',(0.,10.8,4.5));
#12508=CARTESIAN_POINT('',(-1.,1.8,4.5));
#12509=CARTESIAN_POINT('',(-1.,1.8,4.5));
#12510=CARTESIAN_POINT('Origin',(0.,1.8,4.5));
#12511=CARTESIAN_POINT('Origin',(0.,1.8,4.5));
#12512=CARTESIAN_POINT('',(-1.6,10.8,4.5));
#12513=CARTESIAN_POINT('Origin',(0.,10.8,4.5));
#12514=CARTESIAN_POINT('',(-1.6,1.8,4.5));
#12515=CARTESIAN_POINT('',(-1.6,1.8,4.5));
#12516=CARTESIAN_POINT('Origin',(0.,1.8,4.5));
#12517=CARTESIAN_POINT('Origin',(0.,10.8,4.5));
#12518=CARTESIAN_POINT('Origin',(0.,1.8,4.5));
#12519=CARTESIAN_POINT('',(0.,0.,0.));
#12520=CARTESIAN_POINT('Origin',(0.,1.7,4.5));
#12521=CARTESIAN_POINT('',(-1.,1.8,4.5));
#12522=CARTESIAN_POINT('Origin',(0.,1.8,4.5));
#12523=CARTESIAN_POINT('',(-1.,1.7,4.5));
#12524=CARTESIAN_POINT('',(-1.,1.7,4.5));
#12525=CARTESIAN_POINT('Origin',(0.,1.7,4.5));
#12526=CARTESIAN_POINT('Origin',(0.,1.7,4.5));
#12527=CARTESIAN_POINT('',(-1.6,1.8,4.5));
#12528=CARTESIAN_POINT('Origin',(0.,1.8,4.5));
#12529=CARTESIAN_POINT('',(-1.6,1.7,4.5));
#12530=CARTESIAN_POINT('',(-1.6,1.7,4.5));
#12531=CARTESIAN_POINT('Origin',(0.,1.7,4.5));
#12532=CARTESIAN_POINT('Origin',(0.,1.8,4.5));
#12533=CARTESIAN_POINT('Origin',(0.,1.7,4.5));
#12534=CARTESIAN_POINT('',(0.,0.,0.));
#12535=CARTESIAN_POINT('Origin',(0.,10.8,4.5));
#12536=CARTESIAN_POINT('',(-1.,10.9,4.5));
#12537=CARTESIAN_POINT('Origin',(0.,10.9,4.5));
#12538=CARTESIAN_POINT('',(-1.,10.8,4.5));
#12539=CARTESIAN_POINT('',(-1.,10.8,4.5));
#12540=CARTESIAN_POINT('Origin',(0.,10.8,4.5));
#12541=CARTESIAN_POINT('Origin',(0.,10.8,4.5));
#12542=CARTESIAN_POINT('',(-1.6,10.9,4.5));
#12543=CARTESIAN_POINT('Origin',(0.,10.9,4.5));
#12544=CARTESIAN_POINT('',(-1.6,10.8,4.5));
#12545=CARTESIAN_POINT('',(-1.6,10.8,4.5));
#12546=CARTESIAN_POINT('Origin',(0.,10.8,4.5));
#12547=CARTESIAN_POINT('Origin',(0.,10.9,4.5));
#12548=CARTESIAN_POINT('Origin',(0.,10.8,4.5));
#12549=CARTESIAN_POINT('',(0.,0.,0.));
#12550=CARTESIAN_POINT('Origin',(-2.9,0.9,1.4));
#12551=CARTESIAN_POINT('',(-3.35,0.9,1.4));
#12552=CARTESIAN_POINT('Origin',(-2.9,0.9,1.4));
#12553=CARTESIAN_POINT('',(-3.35,0.9,2.));
#12554=CARTESIAN_POINT('',(-3.35,0.9,1.4));
#12555=CARTESIAN_POINT('Origin',(-2.9,0.9,2.));
#12556=CARTESIAN_POINT('Origin',(-2.9,0.9,1.4));
#12557=CARTESIAN_POINT('',(-3.175,0.9,1.4));
#12558=CARTESIAN_POINT('Origin',(-2.9,0.9,1.4));
#12559=CARTESIAN_POINT('Origin',(2.9,0.9,1.4));
#12560=CARTESIAN_POINT('',(2.45,0.9,1.4));
#12561=CARTESIAN_POINT('Origin',(2.9,0.9,1.4));
#12562=CARTESIAN_POINT('',(2.45,0.9,2.));
#12563=CARTESIAN_POINT('',(2.45,0.9,1.4));
#12564=CARTESIAN_POINT('Origin',(2.9,0.9,2.));
#12565=CARTESIAN_POINT('Origin',(2.9,0.9,1.4));
#12566=CARTESIAN_POINT('',(2.625,0.9,1.4));
#12567=CARTESIAN_POINT('Origin',(2.9,0.9,1.4));
#12568=CARTESIAN_POINT('Origin',(-2.9,0.9,-0.1));
#12569=CARTESIAN_POINT('',(-3.175,0.9,0.));
#12570=CARTESIAN_POINT('Origin',(-2.9,0.9,0.));
#12571=CARTESIAN_POINT('',(-3.175,0.9,-0.1));
#12572=CARTESIAN_POINT('Origin',(2.9,0.9,-0.1));
#12573=CARTESIAN_POINT('',(2.625,0.9,0.));
#12574=CARTESIAN_POINT('Origin',(2.9,0.9,0.));
#12575=CARTESIAN_POINT('',(2.625,0.9,-0.1));
#12576=CARTESIAN_POINT('Origin',(-1.2,0.6,-0.1));
#12577=CARTESIAN_POINT('',(-1.7,0.6,0.));
#12578=CARTESIAN_POINT('Origin',(-1.2,0.6,0.));
#12579=CARTESIAN_POINT('',(-1.7,0.6,0.8));
#12580=CARTESIAN_POINT('',(-1.7,0.6,-0.1));
#12581=CARTESIAN_POINT('Origin',(-1.2,0.6,0.8));
#12582=CARTESIAN_POINT('Origin',(-1.2,0.6,0.8));
#12583=CARTESIAN_POINT('',(-1.475,0.6,0.8));
#12584=CARTESIAN_POINT('Origin',(-1.2,0.6,0.8));
#12585=CARTESIAN_POINT('Origin',(1.2,0.6,-0.1));
#12586=CARTESIAN_POINT('',(0.7,0.6,0.));
#12587=CARTESIAN_POINT('Origin',(1.2,0.6,0.));
#12588=CARTESIAN_POINT('',(0.7,0.6,0.8));
#12589=CARTESIAN_POINT('',(0.7,0.6,-0.1));
#12590=CARTESIAN_POINT('Origin',(1.2,0.6,0.8));
#12591=CARTESIAN_POINT('Origin',(1.2,0.6,0.8));
#12592=CARTESIAN_POINT('',(0.925,0.6,0.8));
#12593=CARTESIAN_POINT('Origin',(1.2,0.6,0.8));
#12594=CARTESIAN_POINT('Origin',(-1.2,0.6,-0.1));
#12595=CARTESIAN_POINT('',(-1.475,0.6,2.));
#12596=CARTESIAN_POINT('',(-1.475,0.6,-0.1));
#12597=CARTESIAN_POINT('Origin',(-1.2,0.6,2.));
#12598=CARTESIAN_POINT('Origin',(1.2,0.6,-0.1));
#12599=CARTESIAN_POINT('',(0.925,0.6,2.));
#12600=CARTESIAN_POINT('',(0.925,0.6,-0.1));
#12601=CARTESIAN_POINT('Origin',(1.2,0.6,2.));
#12602=CARTESIAN_POINT('Origin',(3.5,1.8,0.));
#12603=CARTESIAN_POINT('',(3.5,1.8,0.));
#12604=CARTESIAN_POINT('',(-3.5,1.8,0.));
#12605=CARTESIAN_POINT('',(3.5,1.8,0.));
#12606=CARTESIAN_POINT('',(-3.5,1.8,2.));
#12607=CARTESIAN_POINT('',(-3.5,1.8,0.));
#12608=CARTESIAN_POINT('',(3.5,1.8,2.));
#12609=CARTESIAN_POINT('',(3.5,1.8,2.));
#12610=CARTESIAN_POINT('',(3.5,1.8,0.));
#12611=CARTESIAN_POINT('Origin',(3.5,0.,0.));
#12612=CARTESIAN_POINT('',(3.5,0.,0.));
#12613=CARTESIAN_POINT('',(3.5,0.,0.));
#12614=CARTESIAN_POINT('',(3.5,0.,2.));
#12615=CARTESIAN_POINT('',(3.5,0.,2.));
#12616=CARTESIAN_POINT('',(3.5,0.,0.));
#12617=CARTESIAN_POINT('Origin',(-3.5,0.,0.));
#12618=CARTESIAN_POINT('',(-3.5,0.,0.));
#12619=CARTESIAN_POINT('',(-3.5,0.,0.));
#12620=CARTESIAN_POINT('',(-3.5,0.,2.));
#12621=CARTESIAN_POINT('',(-3.5,0.,2.));
#12622=CARTESIAN_POINT('',(-3.5,0.,0.));
#12623=CARTESIAN_POINT('Origin',(-3.5,1.8,0.));
#12624=CARTESIAN_POINT('',(-3.5,1.8,0.));
#12625=CARTESIAN_POINT('',(-3.5,1.8,2.));
#12626=CARTESIAN_POINT('Origin',(0.,0.9,2.));
#12627=CARTESIAN_POINT('Origin',(0.,0.9,0.));
#12628=CARTESIAN_POINT('',(0.,0.,0.));
#12629=CARTESIAN_POINT('Origin',(0.375,0.5,0.));
#12630=CARTESIAN_POINT('',(-0.375,0.5,-4.59242549680257E-17));
#12631=CARTESIAN_POINT('Origin',(0.,0.5,0.));
#12632=CARTESIAN_POINT('Origin',(0.,0.475,0.));
#12633=CARTESIAN_POINT('',(-0.425,0.45,-5.20474889637625E-17));
#12634=CARTESIAN_POINT('Origin',(0.,0.45,0.));
#12635=CARTESIAN_POINT('',(-0.4,0.475,-4.89858719658941E-17));
#12636=CARTESIAN_POINT('Origin',(0.,0.24,0.));
#12637=CARTESIAN_POINT('',(-0.425,0.0299999999999998,-5.20474889637625E-17));
#12638=CARTESIAN_POINT('Origin',(0.,0.0299999999999998,0.));
#12639=CARTESIAN_POINT('',(-0.425,0.24,-5.20474889637625E-17));
#12640=CARTESIAN_POINT('Origin',(0.,0.0150000000000001,0.));
#12641=CARTESIAN_POINT('',(-0.395,4.85722573273506E-17,-4.83735485663204E-17));
#12642=CARTESIAN_POINT('Origin',(0.,0.,0.));
#12643=CARTESIAN_POINT('',(-0.41,0.0150000000000001,-5.02105187650415E-17));
#12644=CARTESIAN_POINT('Origin',(0.27,0.,0.));
#12645=CARTESIAN_POINT('',(-0.27,0.,-3.30654635769785E-17));
#12646=CARTESIAN_POINT('Origin',(0.,0.,0.));
#12647=CARTESIAN_POINT('Origin',(0.,-0.02,0.));
#12648=CARTESIAN_POINT('',(-0.24505,-0.0498999999999999,3.00099698131059E-17));
#12649=CARTESIAN_POINT('Origin',(0.,-0.0498999999999999,0.));
#12650=CARTESIAN_POINT('',(-0.26,-0.02,-3.18408167778312E-17));
#12651=CARTESIAN_POINT('Origin',(0.,-0.995,0.));
#12652=CARTESIAN_POINT('',(-0.24505,-1.95495,3.00099698131059E-17));
#12653=CARTESIAN_POINT('Origin',(0.,-1.95495,0.));
#12654=CARTESIAN_POINT('',(-0.24505,-0.995,-3.00099698131059E-17));
#12655=CARTESIAN_POINT('Origin',(0.,-1.975,0.));
#12656=CARTESIAN_POINT('',(-0.2,-2.,-2.44929359829471E-17));
#12657=CARTESIAN_POINT('Origin',(0.,-2.,0.));
#12658=CARTESIAN_POINT('',(-0.225,-1.975,-2.75545529808154E-17));
#12659=CARTESIAN_POINT('Origin',(0.,-2.,0.));
#12660=CARTESIAN_POINT('Origin',(0.115470053837925,-0.5,-0.2));
#12661=CARTESIAN_POINT('',(0.23094010767585,-0.5,0.));
#12662=CARTESIAN_POINT('',(0.115470053837925,-0.5,-0.2));
#12663=CARTESIAN_POINT('',(0.23094010767585,-0.5,0.));
#12664=CARTESIAN_POINT('',(0.115470053837925,-0.8,-0.2));
#12665=CARTESIAN_POINT('',(0.115470053837925,-0.5,-0.2));
#12666=CARTESIAN_POINT('',(0.23094010767585,-0.8,0.));
#12667=CARTESIAN_POINT('',(0.23094010767585,-0.8,0.));
#12668=CARTESIAN_POINT('',(0.23094010767585,-0.5,0.));
#12669=CARTESIAN_POINT('Origin',(-0.115470053837925,-0.5,-0.2));
#12670=CARTESIAN_POINT('',(-0.115470053837925,-0.5,-0.2));
#12671=CARTESIAN_POINT('',(0.115470053837925,-0.5,-0.2));
#12672=CARTESIAN_POINT('',(-0.115470053837925,-0.8,-0.2));
#12673=CARTESIAN_POINT('',(-0.115470053837925,-0.5,-0.2));
#12674=CARTESIAN_POINT('',(0.115470053837925,-0.8,-0.2));
#12675=CARTESIAN_POINT('Origin',(-0.23094010767585,-0.5,-2.77555756156289E-17));
#12676=CARTESIAN_POINT('',(-0.23094010767585,-0.5,-2.82820063659975E-17));
#12677=CARTESIAN_POINT('',(-0.115470053837925,-0.5,-0.2));
#12678=CARTESIAN_POINT('',(-0.23094010767585,-0.8,-2.77555756156289E-17));
#12679=CARTESIAN_POINT('',(-0.23094010767585,-0.5,-2.82820063659975E-17));
#12680=CARTESIAN_POINT('',(-0.115470053837925,-0.8,-0.2));
#12681=CARTESIAN_POINT('Origin',(-0.115470053837925,-0.5,0.2));
#12682=CARTESIAN_POINT('',(-0.115470053837925,-0.5,0.2));
#12683=CARTESIAN_POINT('',(-0.23094010767585,-0.5,-2.82820063659975E-17));
#12684=CARTESIAN_POINT('',(-0.115470053837925,-0.8,0.2));
#12685=CARTESIAN_POINT('',(-0.115470053837925,-0.5,0.2));
#12686=CARTESIAN_POINT('',(-0.23094010767585,-0.8,-2.82820063659975E-17));
#12687=CARTESIAN_POINT('Origin',(0.115470053837925,-0.5,0.2));
#12688=CARTESIAN_POINT('',(0.115470053837925,-0.5,0.2));
#12689=CARTESIAN_POINT('',(-0.115470053837925,-0.5,0.2));
#12690=CARTESIAN_POINT('',(0.115470053837925,-0.8,0.2));
#12691=CARTESIAN_POINT('',(0.115470053837925,-0.5,0.2));
#12692=CARTESIAN_POINT('',(-0.115470053837925,-0.8,0.2));
#12693=CARTESIAN_POINT('Origin',(0.23094010767585,-0.5,0.));
#12694=CARTESIAN_POINT('',(0.115470053837925,-0.5,0.2));
#12695=CARTESIAN_POINT('',(0.115470053837925,-0.8,0.2));
#12696=CARTESIAN_POINT('Origin',(0.,-0.5,0.));
#12697=CARTESIAN_POINT('Origin',(0.,-0.8,0.));
#12698=CARTESIAN_POINT('',(0.,0.,0.));
#12699=CARTESIAN_POINT('',(0.,0.,0.));
#12700=CARTESIAN_POINT('Origin',(0.,0.6,0.));
#12701=CARTESIAN_POINT('',(-0.43,0.6,5.26598123633362E-17));
#12702=CARTESIAN_POINT('Origin',(0.,0.6,0.));
#12703=CARTESIAN_POINT('',(-0.43,0.7,-5.26598123633362E-17));
#12704=CARTESIAN_POINT('',(-0.43,0.6,5.26598123633362E-17));
#12705=CARTESIAN_POINT('Origin',(0.,0.7,0.));
#12706=CARTESIAN_POINT('Origin',(0.,0.6,0.));
#12707=CARTESIAN_POINT('',(-0.2,0.6,2.44929359829471E-17));
#12708=CARTESIAN_POINT('Origin',(0.,0.6,0.));
#12709=CARTESIAN_POINT('Origin',(0.,0.5,-1.11022302462516E-16));
#12710=CARTESIAN_POINT('',(0.346410161513776,0.5,0.6));
#12711=CARTESIAN_POINT('',(0.692820323027551,0.5,0.));
#12712=CARTESIAN_POINT('',(0.346410161513776,0.5,0.6));
#12713=CARTESIAN_POINT('',(0.346410161513776,0.5,-0.6));
#12714=CARTESIAN_POINT('',(0.692820323027551,0.5,0.));
#12715=CARTESIAN_POINT('',(-0.346410161513775,0.5,-0.6));
#12716=CARTESIAN_POINT('',(0.346410161513776,0.5,-0.6));
#12717=CARTESIAN_POINT('',(-0.692820323027551,0.5,-8.48460190979926E-17));
#12718=CARTESIAN_POINT('',(-0.346410161513775,0.5,-0.6));
#12719=CARTESIAN_POINT('',(-0.346410161513776,0.5,0.6));
#12720=CARTESIAN_POINT('',(-0.692820323027551,0.5,-8.48460190979926E-17));
#12721=CARTESIAN_POINT('',(-0.346410161513776,0.5,0.6));
#12722=CARTESIAN_POINT('',(-0.525,0.5,-6.4293956955236E-17));
#12723=CARTESIAN_POINT('Origin',(0.,0.5,0.));
#12724=CARTESIAN_POINT('Origin',(0.,0.,-1.11022302462516E-16));
#12725=CARTESIAN_POINT('',(0.346410161513776,0.,0.6));
#12726=CARTESIAN_POINT('',(0.692820323027551,0.,0.));
#12727=CARTESIAN_POINT('',(0.346410161513776,0.,0.6));
#12728=CARTESIAN_POINT('',(-0.346410161513776,0.,0.6));
#12729=CARTESIAN_POINT('',(-0.346410161513776,0.,0.6));
#12730=CARTESIAN_POINT('',(-0.692820323027551,0.,-8.48460190979926E-17));
#12731=CARTESIAN_POINT('',(-0.692820323027551,0.,-8.48460190979926E-17));
#12732=CARTESIAN_POINT('',(-0.346410161513775,0.,-0.6));
#12733=CARTESIAN_POINT('',(-0.346410161513775,0.,-0.6));
#12734=CARTESIAN_POINT('',(0.346410161513776,0.,-0.6));
#12735=CARTESIAN_POINT('',(0.346410161513776,0.,-0.6));
#12736=CARTESIAN_POINT('',(0.692820323027551,0.,0.));
#12737=CARTESIAN_POINT('',(-0.515,0.,-6.30693101560887E-17));
#12738=CARTESIAN_POINT('Origin',(0.,0.,0.));
#12739=CARTESIAN_POINT('Origin',(-0.346410161513776,0.,0.6));
#12740=CARTESIAN_POINT('',(0.346410161513776,0.,0.6));
#12741=CARTESIAN_POINT('',(-0.346410161513776,0.,0.6));
#12742=CARTESIAN_POINT('Origin',(-0.692820323027551,0.,-8.48460190979926E-17));
#12743=CARTESIAN_POINT('',(-0.692820323027551,0.,-8.48460190979926E-17));
#12744=CARTESIAN_POINT('Origin',(-0.346410161513775,0.,-0.6));
#12745=CARTESIAN_POINT('',(-0.346410161513775,0.,-0.6));
#12746=CARTESIAN_POINT('Origin',(0.346410161513776,0.,-0.6));
#12747=CARTESIAN_POINT('',(0.346410161513776,0.,-0.6));
#12748=CARTESIAN_POINT('Origin',(0.692820323027551,0.,0.));
#12749=CARTESIAN_POINT('',(0.692820323027551,0.,0.));
#12750=CARTESIAN_POINT('Origin',(0.346410161513776,0.,0.6));
#12751=CARTESIAN_POINT('Origin',(0.46,0.7,0.));
#12752=CARTESIAN_POINT('',(-0.46,0.7,-5.63337527607782E-17));
#12753=CARTESIAN_POINT('Origin',(0.,0.7,0.));
#12754=CARTESIAN_POINT('Origin',(0.,1.2,0.));
#12755=CARTESIAN_POINT('',(-0.46,1.7,-5.63337527607782E-17));
#12756=CARTESIAN_POINT('',(-0.46,1.2,-5.63337527607782E-17));
#12757=CARTESIAN_POINT('Origin',(0.,1.7,0.));
#12758=CARTESIAN_POINT('Origin',(0.525,1.7,0.));
#12759=CARTESIAN_POINT('',(-0.525,1.7,-6.4293956955236E-17));
#12760=CARTESIAN_POINT('Origin',(0.,1.7,0.));
#12761=CARTESIAN_POINT('Origin',(0.,1.1,0.));
#12762=CARTESIAN_POINT('',(-0.525,1.1,-6.4293956955236E-17));
#12763=CARTESIAN_POINT('Origin',(0.,-0.325,0.));
#12764=CARTESIAN_POINT('',(-0.515,-0.65,-6.30693101560887E-17));
#12765=CARTESIAN_POINT('Origin',(0.,-0.65,0.));
#12766=CARTESIAN_POINT('',(-0.515,-0.325,-6.30693101560887E-17));
#12767=CARTESIAN_POINT('Origin',(0.2,-0.65,0.));
#12768=CARTESIAN_POINT('',(-0.2,-0.65,-2.44929359829471E-17));
#12769=CARTESIAN_POINT('Origin',(0.,-0.65,0.));
#12770=CARTESIAN_POINT('Origin',(0.,0.0249999999999999,0.));
#12771=CARTESIAN_POINT('',(-0.2,0.0249999999999999,-2.44929359829471E-17));
#12772=CARTESIAN_POINT('',(0.,0.,0.));
#12773=CARTESIAN_POINT('Origin',(0.475,1.95,0.));
#12774=CARTESIAN_POINT('',(-0.475,1.95,-5.81707229594993E-17));
#12775=CARTESIAN_POINT('Origin',(0.,1.95,0.));
#12776=CARTESIAN_POINT('',(-0.31,1.95,-3.7964050773568E-17));
#12777=CARTESIAN_POINT('Origin',(0.,1.95,0.));
#12778=CARTESIAN_POINT('Origin',(0.,1.825,0.));
#12779=CARTESIAN_POINT('',(-0.475,1.7,-5.81707229594993E-17));
#12780=CARTESIAN_POINT('Origin',(0.,1.7,0.));
#12781=CARTESIAN_POINT('',(-0.475,1.825,-5.81707229594993E-17));
#12782=CARTESIAN_POINT('Origin',(0.355,1.7,0.));
#12783=CARTESIAN_POINT('',(-0.355,1.7,-4.3474961369731E-17));
#12784=CARTESIAN_POINT('Origin',(0.,1.7,0.));
#12785=CARTESIAN_POINT('Origin',(0.,1.55,0.));
#12786=CARTESIAN_POINT('',(-0.355,1.4,-4.3474961369731E-17));
#12787=CARTESIAN_POINT('Origin',(0.,1.4,0.));
#12788=CARTESIAN_POINT('',(-0.355,1.55,-4.3474961369731E-17));
#12789=CARTESIAN_POINT('Origin',(0.31,1.4,0.));
#12790=CARTESIAN_POINT('',(-0.31,1.4,-3.7964050773568E-17));
#12791=CARTESIAN_POINT('Origin',(0.,1.4,0.));
#12792=CARTESIAN_POINT('Origin',(0.,1.675,0.));
#12793=CARTESIAN_POINT('',(-0.31,1.675,-3.7964050773568E-17));
#12794=CARTESIAN_POINT('',(0.,0.,0.));
#12795=CARTESIAN_POINT('',(0.,0.,0.));
#12796=CARTESIAN_POINT('',(0.,0.,0.));
#12797=CARTESIAN_POINT('Origin',(0.,0.,0.));
#12798=CARTESIAN_POINT('',(-3.71680303541222E-17,-1.08993565124114E-17,
0.3035));
#12799=CARTESIAN_POINT('Origin',(-4.80673868665336E-17,0.,0.3925));
#12800=CARTESIAN_POINT('Origin',(0.,1.08993565124114E-17,0.));
#12801=CARTESIAN_POINT('',(0.,0.,0.));
#12802=CARTESIAN_POINT('Origin',(0.,0.125,4.5));
#12803=CARTESIAN_POINT('',(-0.51,0.125,4.5));
#12804=CARTESIAN_POINT('Origin',(0.,0.125,4.5));
#12805=CARTESIAN_POINT('',(-0.51,0.275,4.5));
#12806=CARTESIAN_POINT('',(-0.51,0.125,4.5));
#12807=CARTESIAN_POINT('Origin',(0.,0.275,4.5));
#12808=CARTESIAN_POINT('Origin',(0.,0.275,4.5));
#12809=CARTESIAN_POINT('',(-0.405,0.275,4.5));
#12810=CARTESIAN_POINT('Origin',(0.,0.275,4.5));
#12811=CARTESIAN_POINT('Origin',(0.,0.125,4.5));
#12812=CARTESIAN_POINT('',(-0.405,0.125,4.5));
#12813=CARTESIAN_POINT('Origin',(0.,0.125,4.5));
#12814=CARTESIAN_POINT('Origin',(0.,0.,4.5));
#12815=CARTESIAN_POINT('',(-0.405,0.,4.5));
#12816=CARTESIAN_POINT('',(-0.405,0.,4.5));
#12817=CARTESIAN_POINT('Origin',(0.,0.,4.5));
#12818=CARTESIAN_POINT('Origin',(0.,0.,4.5));
#12819=CARTESIAN_POINT('',(-0.405,1.2,4.5));
#12820=CARTESIAN_POINT('Origin',(0.,1.2,4.5));
#12821=CARTESIAN_POINT('',(-0.405,0.,4.5));
#12822=CARTESIAN_POINT('Origin',(0.,0.,4.5));
#12823=CARTESIAN_POINT('',(-0.6,1.2,4.5));
#12824=CARTESIAN_POINT('Origin',(0.,1.2,4.5));
#12825=CARTESIAN_POINT('',(-0.6,0.,4.5));
#12826=CARTESIAN_POINT('',(-0.6,0.,4.5));
#12827=CARTESIAN_POINT('Origin',(0.,0.,4.5));
#12828=CARTESIAN_POINT('Origin',(0.,1.2,4.5));
#12829=CARTESIAN_POINT('Origin',(0.,0.,4.5));
#12830=CARTESIAN_POINT('',(0.,0.,0.));
#12831=CARTESIAN_POINT('Origin',(0.,0.2,4.5));
#12832=CARTESIAN_POINT('',(-4.89858719658941E-17,0.2,4.9));
#12833=CARTESIAN_POINT('Origin',(-5.51091059616309E-17,0.2,4.95));
#12834=CARTESIAN_POINT('Origin',(0.,0.2,4.5));
#12835=CARTESIAN_POINT('',(0.,0.,0.));
#12836=CARTESIAN_POINT('Origin',(-2.,-1.,2.5));
#12837=CARTESIAN_POINT('',(-2.25,13.6,2.5));
#12838=CARTESIAN_POINT('Origin',(-2.,13.6,2.5));
#12839=CARTESIAN_POINT('',(-2.25,-1.,2.5));
#12840=CARTESIAN_POINT('',(-2.25,-1.,2.5));
#12841=CARTESIAN_POINT('Origin',(-2.,-1.,2.5));
#12842=CARTESIAN_POINT('Origin',(-2.,13.6,2.5));
#12843=CARTESIAN_POINT('Origin',(-2.,-1.,2.5));
#12844=CARTESIAN_POINT('',(0.,0.,0.));
#12845=CARTESIAN_POINT('Origin',(0.,0.09,0.));
#12846=CARTESIAN_POINT('',(-0.285,0.1,3.49024337756996E-17));
#12847=CARTESIAN_POINT('Origin',(0.,0.1,0.));
#12848=CARTESIAN_POINT('',(-0.265,0.08,-3.24531401774049E-17));
#12849=CARTESIAN_POINT('',(-0.275,0.09,3.36777869765522E-17));
#12850=CARTESIAN_POINT('Origin',(0.,0.08,0.));
#12851=CARTESIAN_POINT('Origin',(0.,0.,0.));
#12852=CARTESIAN_POINT('',(-0.265,0.,3.24531401774049E-17));
#12853=CARTESIAN_POINT('',(-0.265,0.,3.24531401774049E-17));
#12854=CARTESIAN_POINT('Origin',(0.,0.,0.));
#12855=CARTESIAN_POINT('Origin',(0.,0.1,0.));
#12856=CARTESIAN_POINT('',(-0.5,0.1,6.12323399573677E-17));
#12857=CARTESIAN_POINT('Origin',(0.,0.1,0.));
#12858=CARTESIAN_POINT('Origin',(0.,0.,0.));
#12859=CARTESIAN_POINT('',(-0.5,0.,6.12323399573677E-17));
#12860=CARTESIAN_POINT('',(-0.5,0.,6.12323399573677E-17));
#12861=CARTESIAN_POINT('Origin',(0.,0.,0.));
#12862=CARTESIAN_POINT('Origin',(0.,0.,0.));
#12863=CARTESIAN_POINT('',(0.,0.,0.));
#12864=CARTESIAN_POINT('Origin',(0.,0.0525042956467857,0.));
#12865=CARTESIAN_POINT('',(-0.230940107675851,0.0472735643746089,0.4));
#12866=CARTESIAN_POINT('',(0.23094010767585,0.0472735643746089,0.4));
#12867=CARTESIAN_POINT('Ctrl Pts',(-0.230940107675851,0.0472735643746089,
0.4));
#12868=CARTESIAN_POINT('Ctrl Pts',(1.11022302462516E-16,-0.0193931022920578,
0.4));
#12869=CARTESIAN_POINT('Ctrl Pts',(0.23094010767585,0.0472735643746089,
0.4));
#12870=CARTESIAN_POINT('',(-0.461880215351701,0.0472735643746089,-5.6564012731995E-17));
#12871=CARTESIAN_POINT('Ctrl Pts',(-0.461880215351701,0.0472735643746089,
-5.6564012731995E-17));
#12872=CARTESIAN_POINT('Ctrl Pts',(-0.346410161513776,-0.0193931022920579,
0.2));
#12873=CARTESIAN_POINT('Ctrl Pts',(-0.230940107675851,0.0472735643746089,
0.4));
#12874=CARTESIAN_POINT('',(-0.38,-2.08166817117217E-17,-4.65365783675994E-17));
#12875=CARTESIAN_POINT('',(-0.47094010767585,0.0525042956467857,-5.7673529545534E-17));
#12876=CARTESIAN_POINT('Origin',(0.,0.,0.));
#12877=CARTESIAN_POINT('',(-0.23094010767585,0.0472735643746089,-0.4));
#12878=CARTESIAN_POINT('Ctrl Pts',(-0.23094010767585,0.0472735643746089,
-0.4));
#12879=CARTESIAN_POINT('Ctrl Pts',(-0.346410161513775,-0.0193931022920578,
-0.2));
#12880=CARTESIAN_POINT('Ctrl Pts',(-0.461880215351701,0.0472735643746089,
-5.6564012731995E-17));
#12881=CARTESIAN_POINT('',(0.23094010767585,0.0472735643746089,-0.4));
#12882=CARTESIAN_POINT('Ctrl Pts',(0.23094010767585,0.0472735643746089,
-0.4));
#12883=CARTESIAN_POINT('Ctrl Pts',(0.,-0.0193931022920578,-0.4));
#12884=CARTESIAN_POINT('Ctrl Pts',(-0.23094010767585,0.0472735643746089,
-0.4));
#12885=CARTESIAN_POINT('',(0.461880215351701,0.0472735643746089,0.));
#12886=CARTESIAN_POINT('Ctrl Pts',(0.461880215351701,0.0472735643746089,
0.));
#12887=CARTESIAN_POINT('Ctrl Pts',(0.346410161513776,-0.019393102292058,
-0.2));
#12888=CARTESIAN_POINT('Ctrl Pts',(0.23094010767585,0.0472735643746089,
-0.4));
#12889=CARTESIAN_POINT('Ctrl Pts',(0.23094010767585,0.0472735643746089,
0.4));
#12890=CARTESIAN_POINT('Ctrl Pts',(0.346410161513776,-0.0193931022920577,
0.2));
#12891=CARTESIAN_POINT('Ctrl Pts',(0.461880215351701,0.0472735643746089,
0.));
#12892=CARTESIAN_POINT('Origin',(0.,0.417495704353214,0.));
#12893=CARTESIAN_POINT('',(-0.38,0.47,-4.65365783675994E-17));
#12894=CARTESIAN_POINT('Origin',(0.,0.47,0.));
#12895=CARTESIAN_POINT('',(-0.461880215351701,0.422726435625391,-5.6564012731995E-17));
#12896=CARTESIAN_POINT('',(-0.47094010767585,0.417495704353214,-5.7673529545534E-17));
#12897=CARTESIAN_POINT('',(-0.230940107675851,0.422726435625391,0.4));
#12898=CARTESIAN_POINT('Ctrl Pts',(-0.230940107675851,0.422726435625391,
0.4));
#12899=CARTESIAN_POINT('Ctrl Pts',(-0.346410161513776,0.489393102292058,
0.2));
#12900=CARTESIAN_POINT('Ctrl Pts',(-0.461880215351701,0.422726435625391,
-5.6564012731995E-17));
#12901=CARTESIAN_POINT('',(0.23094010767585,0.422726435625391,0.4));
#12902=CARTESIAN_POINT('Ctrl Pts',(0.23094010767585,0.422726435625391,0.4));
#12903=CARTESIAN_POINT('Ctrl Pts',(8.32667268468867E-17,0.489393102292058,
0.4));
#12904=CARTESIAN_POINT('Ctrl Pts',(-0.230940107675851,0.422726435625391,
0.4));
#12905=CARTESIAN_POINT('',(0.461880215351701,0.422726435625391,0.));
#12906=CARTESIAN_POINT('Ctrl Pts',(0.461880215351701,0.422726435625391,
0.));
#12907=CARTESIAN_POINT('Ctrl Pts',(0.346410161513776,0.489393102292058,
0.2));
#12908=CARTESIAN_POINT('Ctrl Pts',(0.23094010767585,0.422726435625391,0.4));
#12909=CARTESIAN_POINT('',(0.23094010767585,0.422726435625391,-0.4));
#12910=CARTESIAN_POINT('Ctrl Pts',(0.23094010767585,0.422726435625391,-0.4));
#12911=CARTESIAN_POINT('Ctrl Pts',(0.346410161513775,0.489393102292058,
-0.2));
#12912=CARTESIAN_POINT('Ctrl Pts',(0.461880215351701,0.422726435625391,
0.));
#12913=CARTESIAN_POINT('',(-0.23094010767585,0.422726435625391,-0.4));
#12914=CARTESIAN_POINT('Ctrl Pts',(-0.23094010767585,0.422726435625391,
-0.4));
#12915=CARTESIAN_POINT('Ctrl Pts',(-5.55111512312578E-17,0.489393102292058,
-0.4));
#12916=CARTESIAN_POINT('Ctrl Pts',(0.23094010767585,0.422726435625391,-0.4));
#12917=CARTESIAN_POINT('Ctrl Pts',(-0.461880215351701,0.422726435625391,
-5.6564012731995E-17));
#12918=CARTESIAN_POINT('Ctrl Pts',(-0.346410161513776,0.489393102292058,
-0.2));
#12919=CARTESIAN_POINT('Ctrl Pts',(-0.23094010767585,0.422726435625391,
-0.4));
#12920=CARTESIAN_POINT('Origin',(0.23094010767585,0.,-0.4));
#12921=CARTESIAN_POINT('',(-0.23094010767585,0.,-0.4));
#12922=CARTESIAN_POINT('',(0.23094010767585,0.,-0.4));
#12923=CARTESIAN_POINT('Origin',(-0.23094010767585,0.,-0.4));
#12924=CARTESIAN_POINT('',(-0.461880215351701,0.,-5.6564012731995E-17));
#12925=CARTESIAN_POINT('Origin',(-0.461880215351701,0.,-5.6564012731995E-17));
#12926=CARTESIAN_POINT('',(-0.230940107675851,0.,0.4));
#12927=CARTESIAN_POINT('Origin',(0.,0.,0.));
#12928=CARTESIAN_POINT('',(-0.2117,0.47,2.59257727379495E-17));
#12929=CARTESIAN_POINT('Origin',(0.,0.47,0.));
#12930=CARTESIAN_POINT('',(-0.2117,0.,2.59257727379495E-17));
#12931=CARTESIAN_POINT('',(-0.2117,0.,2.59257727379495E-17));
#12932=CARTESIAN_POINT('Origin',(0.,0.,0.));
#12933=CARTESIAN_POINT('Origin',(-0.230940107675851,0.,0.4));
#12934=CARTESIAN_POINT('',(0.23094010767585,0.,0.4));
#12935=CARTESIAN_POINT('Origin',(0.461880215351701,0.,0.));
#12936=CARTESIAN_POINT('',(0.461880215351701,0.,0.));
#12937=CARTESIAN_POINT('Origin',(0.23094010767585,0.,0.4));
#12938=CARTESIAN_POINT('Origin',(0.,0.47,0.));
#12939=CARTESIAN_POINT('Origin',(0.,0.,0.));
#12940=CARTESIAN_POINT('',(0.,0.,0.));
#12941=CARTESIAN_POINT('Origin',(5.7,-4.,-0.9));
#12942=CARTESIAN_POINT('',(5.37,-4.,-0.8));
#12943=CARTESIAN_POINT('Origin',(5.7,-4.,-0.8));
#12944=CARTESIAN_POINT('',(5.37,-4.,0.));
#12945=CARTESIAN_POINT('',(5.37,-4.,-0.9));
#12946=CARTESIAN_POINT('Origin',(5.7,-4.,0.));
#12947=CARTESIAN_POINT('Origin',(-5.7,12.5,-0.9));
#12948=CARTESIAN_POINT('',(-6.03,12.5,-0.8));
#12949=CARTESIAN_POINT('Origin',(-5.7,12.5,-0.8));
#12950=CARTESIAN_POINT('',(-6.03,12.5,0.));
#12951=CARTESIAN_POINT('',(-6.03,12.5,-0.9));
#12952=CARTESIAN_POINT('Origin',(-5.7,12.5,0.));
#12953=CARTESIAN_POINT('Origin',(-5.7,-4.,-0.9));
#12954=CARTESIAN_POINT('',(-6.03,-4.,-0.8));
#12955=CARTESIAN_POINT('Origin',(-5.7,-4.,-0.8));
#12956=CARTESIAN_POINT('',(-6.03,-4.,0.));
#12957=CARTESIAN_POINT('',(-6.03,-4.,-0.9));
#12958=CARTESIAN_POINT('Origin',(-5.7,-4.,0.));
#12959=CARTESIAN_POINT('Origin',(5.7,12.5,-0.9));
#12960=CARTESIAN_POINT('',(5.37,12.5,-0.8));
#12961=CARTESIAN_POINT('Origin',(5.7,12.5,-0.8));
#12962=CARTESIAN_POINT('',(5.37,12.5,0.));
#12963=CARTESIAN_POINT('',(5.37,12.5,-0.9));
#12964=CARTESIAN_POINT('Origin',(5.7,12.5,0.));
#12965=CARTESIAN_POINT('Origin',(2.9,11.7,-0.9));
#12966=CARTESIAN_POINT('',(2.69,11.7,-0.8));
#12967=CARTESIAN_POINT('Origin',(2.9,11.7,-0.8));
#12968=CARTESIAN_POINT('',(2.69,11.7,0.));
#12969=CARTESIAN_POINT('',(2.69,11.7,-0.9));
#12970=CARTESIAN_POINT('Origin',(2.9,11.7,0.));
#12971=CARTESIAN_POINT('Origin',(2.9,0.9,-0.9));
#12972=CARTESIAN_POINT('',(2.69,0.9,-0.8));
#12973=CARTESIAN_POINT('Origin',(2.9,0.9,-0.8));
#12974=CARTESIAN_POINT('',(2.69,0.9,0.));
#12975=CARTESIAN_POINT('',(2.69,0.9,-0.9));
#12976=CARTESIAN_POINT('Origin',(2.9,0.9,0.));
#12977=CARTESIAN_POINT('Origin',(-2.9,11.7,-0.9));
#12978=CARTESIAN_POINT('',(-3.11,11.7,-0.8));
#12979=CARTESIAN_POINT('Origin',(-2.9,11.7,-0.8));
#12980=CARTESIAN_POINT('',(-3.11,11.7,0.));
#12981=CARTESIAN_POINT('',(-3.11,11.7,-0.9));
#12982=CARTESIAN_POINT('Origin',(-2.9,11.7,0.));
#12983=CARTESIAN_POINT('Origin',(-2.9,0.9,-0.9));
#12984=CARTESIAN_POINT('',(-3.11,0.9,-0.8));
#12985=CARTESIAN_POINT('Origin',(-2.9,0.9,-0.8));
#12986=CARTESIAN_POINT('',(-3.11,0.9,0.));
#12987=CARTESIAN_POINT('',(-3.11,0.9,-0.9));
#12988=CARTESIAN_POINT('Origin',(-2.9,0.9,0.));
#12989=CARTESIAN_POINT('Origin',(3.86862915010152,5.9,3.36862915010152));
#12990=CARTESIAN_POINT('',(3.70362915010152,6.,3.36862915010152));
#12991=CARTESIAN_POINT('Origin',(3.86862915010152,6.,3.36862915010152));
#12992=CARTESIAN_POINT('',(3.70362915010152,9.,3.36862915010152));
#12993=CARTESIAN_POINT('',(3.70362915010152,5.9,3.36862915010152));
#12994=CARTESIAN_POINT('Origin',(3.86862915010152,9.,3.36862915010152));
#12995=CARTESIAN_POINT('Origin',(3.86862915010152,5.9,5.63137084989848));
#12996=CARTESIAN_POINT('',(3.70362915010152,6.,5.63137084989848));
#12997=CARTESIAN_POINT('Origin',(3.86862915010152,6.,5.63137084989848));
#12998=CARTESIAN_POINT('',(3.70362915010152,9.,5.63137084989848));
#12999=CARTESIAN_POINT('',(3.70362915010152,5.9,5.63137084989848));
#13000=CARTESIAN_POINT('Origin',(3.86862915010152,9.,5.63137084989848));
#13001=CARTESIAN_POINT('Origin',(6.13137084989848,5.9,5.63137084989848));
#13002=CARTESIAN_POINT('',(5.96637084989848,6.,5.63137084989848));
#13003=CARTESIAN_POINT('Origin',(6.13137084989848,6.,5.63137084989848));
#13004=CARTESIAN_POINT('',(5.96637084989848,9.,5.63137084989848));
#13005=CARTESIAN_POINT('',(5.96637084989848,5.9,5.63137084989848));
#13006=CARTESIAN_POINT('Origin',(6.13137084989848,9.,5.63137084989848));
#13007=CARTESIAN_POINT('Origin',(6.13137084989848,5.9,3.36862915010152));
#13008=CARTESIAN_POINT('',(5.96637084989848,6.,3.36862915010152));
#13009=CARTESIAN_POINT('Origin',(6.13137084989848,6.,3.36862915010152));
#13010=CARTESIAN_POINT('',(5.96637084989848,9.,3.36862915010152));
#13011=CARTESIAN_POINT('',(5.96637084989848,5.9,3.36862915010152));
#13012=CARTESIAN_POINT('Origin',(6.13137084989848,9.,3.36862915010152));
#13013=CARTESIAN_POINT('Origin',(5.,5.9,4.5));
#13014=CARTESIAN_POINT('',(3.95,6.,4.5));
#13015=CARTESIAN_POINT('Origin',(5.,6.,4.5));
#13016=CARTESIAN_POINT('',(3.95,9.,4.5));
#13017=CARTESIAN_POINT('',(3.95,5.9,4.5));
#13018=CARTESIAN_POINT('Origin',(5.,9.,4.5));
#13019=CARTESIAN_POINT('Origin',(3.,6.,0.));
#13020=CARTESIAN_POINT('',(3.,6.,6.5));
#13021=CARTESIAN_POINT('',(3.,6.,0.));
#13022=CARTESIAN_POINT('',(3.,6.,6.5));
#13023=CARTESIAN_POINT('',(3.,9.,6.5));
#13024=CARTESIAN_POINT('',(3.,6.,6.5));
#13025=CARTESIAN_POINT('',(3.,9.,0.));
#13026=CARTESIAN_POINT('',(3.,9.,6.5));
#13027=CARTESIAN_POINT('',(3.,5.25,0.));
#13028=CARTESIAN_POINT('Origin',(7.,6.,6.5));
#13029=CARTESIAN_POINT('',(7.,6.,0.));
#13030=CARTESIAN_POINT('',(7.,6.,6.5));
#13031=CARTESIAN_POINT('',(7.,6.,0.));
#13032=CARTESIAN_POINT('',(7.,9.,0.));
#13033=CARTESIAN_POINT('',(7.,5.25,0.));
#13034=CARTESIAN_POINT('',(7.,9.,6.5));
#13035=CARTESIAN_POINT('',(7.,9.,0.));
#13036=CARTESIAN_POINT('',(7.,6.,6.5));
#13037=CARTESIAN_POINT('Origin',(3.,6.,6.5));
#13038=CARTESIAN_POINT('',(7.,6.,6.5));
#13039=CARTESIAN_POINT('',(7.,9.,6.5));
#13040=CARTESIAN_POINT('Origin',(5.,9.,3.25));
#13041=CARTESIAN_POINT('',(2.5,9.,0.));
#13042=CARTESIAN_POINT('Origin',(5.,6.,3.25));
#13043=CARTESIAN_POINT('',(2.5,6.,0.));
#13044=CARTESIAN_POINT('Origin',(-6.13137084989848,5.9,3.36862915010152));
#13045=CARTESIAN_POINT('',(-6.29637084989848,6.,3.36862915010152));
#13046=CARTESIAN_POINT('Origin',(-6.13137084989848,6.,3.36862915010152));
#13047=CARTESIAN_POINT('',(-6.29637084989848,9.,3.36862915010152));
#13048=CARTESIAN_POINT('',(-6.29637084989848,5.9,3.36862915010152));
#13049=CARTESIAN_POINT('Origin',(-6.13137084989848,9.,3.36862915010152));
#13050=CARTESIAN_POINT('Origin',(-6.13137084989848,5.9,5.63137084989848));
#13051=CARTESIAN_POINT('',(-6.29637084989848,6.,5.63137084989848));
#13052=CARTESIAN_POINT('Origin',(-6.13137084989848,6.,5.63137084989848));
#13053=CARTESIAN_POINT('',(-6.29637084989848,9.,5.63137084989848));
#13054=CARTESIAN_POINT('',(-6.29637084989848,5.9,5.63137084989848));
#13055=CARTESIAN_POINT('Origin',(-6.13137084989848,9.,5.63137084989848));
#13056=CARTESIAN_POINT('Origin',(-3.86862915010152,5.9,5.63137084989848));
#13057=CARTESIAN_POINT('',(-4.03362915010152,6.,5.63137084989848));
#13058=CARTESIAN_POINT('Origin',(-3.86862915010152,6.,5.63137084989848));
#13059=CARTESIAN_POINT('',(-4.03362915010152,9.,5.63137084989848));
#13060=CARTESIAN_POINT('',(-4.03362915010152,5.9,5.63137084989848));
#13061=CARTESIAN_POINT('Origin',(-3.86862915010152,9.,5.63137084989848));
#13062=CARTESIAN_POINT('Origin',(-3.86862915010152,5.9,3.36862915010152));
#13063=CARTESIAN_POINT('',(-4.03362915010152,6.,3.36862915010152));
#13064=CARTESIAN_POINT('Origin',(-3.86862915010152,6.,3.36862915010152));
#13065=CARTESIAN_POINT('',(-4.03362915010152,9.,3.36862915010152));
#13066=CARTESIAN_POINT('',(-4.03362915010152,5.9,3.36862915010152));
#13067=CARTESIAN_POINT('Origin',(-3.86862915010152,9.,3.36862915010152));
#13068=CARTESIAN_POINT('Origin',(-5.,5.9,4.5));
#13069=CARTESIAN_POINT('',(-6.05,6.,4.5));
#13070=CARTESIAN_POINT('Origin',(-5.,6.,4.5));
#13071=CARTESIAN_POINT('',(-6.05,9.,4.5));
#13072=CARTESIAN_POINT('',(-6.05,5.9,4.5));
#13073=CARTESIAN_POINT('Origin',(-5.,9.,4.5));
#13074=CARTESIAN_POINT('Origin',(-7.,6.,0.));
#13075=CARTESIAN_POINT('',(-7.,6.,6.5));
#13076=CARTESIAN_POINT('',(-7.,6.,0.));
#13077=CARTESIAN_POINT('',(-7.,6.,6.5));
#13078=CARTESIAN_POINT('',(-7.,9.,6.5));
#13079=CARTESIAN_POINT('',(-7.,6.,6.5));
#13080=CARTESIAN_POINT('',(-7.,9.,0.));
#13081=CARTESIAN_POINT('',(-7.,9.,6.5));
#13082=CARTESIAN_POINT('',(-7.,5.25,0.));
#13083=CARTESIAN_POINT('Origin',(-3.,6.,6.5));
#13084=CARTESIAN_POINT('',(-3.,6.,0.));
#13085=CARTESIAN_POINT('',(-3.,6.,6.5));
#13086=CARTESIAN_POINT('',(-3.,6.,0.));
#13087=CARTESIAN_POINT('',(-3.,9.,0.));
#13088=CARTESIAN_POINT('',(-3.,5.25,0.));
#13089=CARTESIAN_POINT('',(-3.,9.,6.5));
#13090=CARTESIAN_POINT('',(-3.,9.,0.));
#13091=CARTESIAN_POINT('',(-3.,6.,6.5));
#13092=CARTESIAN_POINT('Origin',(-7.,6.,6.5));
#13093=CARTESIAN_POINT('',(-3.,6.,6.5));
#13094=CARTESIAN_POINT('',(-3.,9.,6.5));
#13095=CARTESIAN_POINT('Origin',(-5.,9.,3.25));
#13096=CARTESIAN_POINT('',(-2.5,9.,0.));
#13097=CARTESIAN_POINT('Origin',(-5.,6.,3.25));
#13098=CARTESIAN_POINT('',(-2.5,6.,0.));
#13099=CARTESIAN_POINT('Origin',(7.5,13.5,-0.8));
#13100=CARTESIAN_POINT('',(7.5,13.5,-0.8));
#13101=CARTESIAN_POINT('',(-7.5,13.5,-0.8));
#13102=CARTESIAN_POINT('',(7.5,13.5,-0.8));
#13103=CARTESIAN_POINT('',(-7.5,13.5,0.));
#13104=CARTESIAN_POINT('',(-7.5,13.5,-0.8));
#13105=CARTESIAN_POINT('',(7.5,13.5,0.));
#13106=CARTESIAN_POINT('',(7.5,13.5,0.));
#13107=CARTESIAN_POINT('',(7.5,13.5,-0.8));
#13108=CARTESIAN_POINT('Origin',(7.5,-4.5,-0.8));
#13109=CARTESIAN_POINT('',(7.5,-4.5,-0.8));
#13110=CARTESIAN_POINT('',(7.5,-4.5,-0.8));
#13111=CARTESIAN_POINT('',(7.5,-4.5,0.));
#13112=CARTESIAN_POINT('',(7.5,-4.5,0.));
#13113=CARTESIAN_POINT('',(7.5,-4.5,-0.8));
#13114=CARTESIAN_POINT('Origin',(-7.5,-4.5,-0.8));
#13115=CARTESIAN_POINT('',(-7.5,-4.5,-0.8));
#13116=CARTESIAN_POINT('',(-7.5,-4.5,-0.8));
#13117=CARTESIAN_POINT('',(-7.5,-4.5,0.));
#13118=CARTESIAN_POINT('',(-7.5,-4.5,0.));
#13119=CARTESIAN_POINT('',(-7.5,-4.5,-0.8));
#13120=CARTESIAN_POINT('Origin',(-7.5,13.5,-0.8));
#13121=CARTESIAN_POINT('',(-7.5,13.5,-0.8));
#13122=CARTESIAN_POINT('',(-7.5,13.5,0.));
#13123=CARTESIAN_POINT('Origin',(0.,4.5,0.));
#13124=CARTESIAN_POINT('Origin',(0.,4.5,-0.8));
#13125=CARTESIAN_POINT('',(0.,0.,0.));
#13126=CARTESIAN_POINT('Origin',(-6.13137084989848,5.6,3.36862915010152));
#13127=CARTESIAN_POINT('',(-6.35637084989848,5.7,3.36862915010152));
#13128=CARTESIAN_POINT('Origin',(-6.13137084989848,5.7,3.36862915010152));
#13129=CARTESIAN_POINT('',(-6.35637084989848,6.,3.36862915010152));
#13130=CARTESIAN_POINT('',(-6.35637084989848,5.6,3.36862915010152));
#13131=CARTESIAN_POINT('Origin',(-6.13137084989848,6.,3.36862915010152));
#13132=CARTESIAN_POINT('Origin',(-6.13137084989848,5.6,5.63137084989848));
#13133=CARTESIAN_POINT('',(-6.35637084989848,5.7,5.63137084989848));
#13134=CARTESIAN_POINT('Origin',(-6.13137084989848,5.7,5.63137084989848));
#13135=CARTESIAN_POINT('',(-6.35637084989848,6.,5.63137084989848));
#13136=CARTESIAN_POINT('',(-6.35637084989848,5.6,5.63137084989848));
#13137=CARTESIAN_POINT('Origin',(-6.13137084989848,6.,5.63137084989848));
#13138=CARTESIAN_POINT('Origin',(-3.86862915010152,5.6,5.63137084989848));
#13139=CARTESIAN_POINT('',(-4.09362915010152,5.7,5.63137084989848));
#13140=CARTESIAN_POINT('Origin',(-3.86862915010152,5.7,5.63137084989848));
#13141=CARTESIAN_POINT('',(-4.09362915010152,6.,5.63137084989848));
#13142=CARTESIAN_POINT('',(-4.09362915010152,5.6,5.63137084989848));
#13143=CARTESIAN_POINT('Origin',(-3.86862915010152,6.,5.63137084989848));
#13144=CARTESIAN_POINT('Origin',(-3.86862915010152,5.6,3.36862915010152));
#13145=CARTESIAN_POINT('',(-4.09362915010152,5.7,3.36862915010152));
#13146=CARTESIAN_POINT('Origin',(-3.86862915010152,5.7,3.36862915010152));
#13147=CARTESIAN_POINT('',(-4.09362915010152,6.,3.36862915010152));
#13148=CARTESIAN_POINT('',(-4.09362915010152,5.6,3.36862915010152));
#13149=CARTESIAN_POINT('Origin',(-3.86862915010152,6.,3.36862915010152));
#13150=CARTESIAN_POINT('Origin',(-5.,5.7,4.5));
#13151=CARTESIAN_POINT('',(-5.62,6.,4.5));
#13152=CARTESIAN_POINT('Origin',(-5.,6.,4.5));
#13153=CARTESIAN_POINT('',(-5.62,5.7,4.5));
#13154=CARTESIAN_POINT('',(-5.62,5.7,4.5));
#13155=CARTESIAN_POINT('Origin',(-5.,5.7,4.5));
#13156=CARTESIAN_POINT('Origin',(-5.,5.7,4.5));
#13157=CARTESIAN_POINT('',(-7.,6.,4.5));
#13158=CARTESIAN_POINT('Origin',(-5.,6.,4.5));
#13159=CARTESIAN_POINT('',(-7.,5.7,4.5));
#13160=CARTESIAN_POINT('',(-7.,5.7,4.5));
#13161=CARTESIAN_POINT('Origin',(-5.,5.7,4.5));
#13162=CARTESIAN_POINT('Origin',(-5.,6.,4.5));
#13163=CARTESIAN_POINT('Origin',(-5.,5.7,4.5));
#13164=CARTESIAN_POINT('',(0.,0.,0.));
#13165=CARTESIAN_POINT('Origin',(-6.13137084989848,8.9,3.36862915010152));
#13166=CARTESIAN_POINT('',(-6.35637084989848,9.,3.36862915010152));
#13167=CARTESIAN_POINT('Origin',(-6.13137084989848,9.,3.36862915010152));
#13168=CARTESIAN_POINT('',(-6.35637084989848,9.3,3.36862915010152));
#13169=CARTESIAN_POINT('',(-6.35637084989848,8.9,3.36862915010152));
#13170=CARTESIAN_POINT('Origin',(-6.13137084989848,9.3,3.36862915010152));
#13171=CARTESIAN_POINT('Origin',(-6.13137084989848,8.9,5.63137084989848));
#13172=CARTESIAN_POINT('',(-6.35637084989848,9.,5.63137084989848));
#13173=CARTESIAN_POINT('Origin',(-6.13137084989848,9.,5.63137084989848));
#13174=CARTESIAN_POINT('',(-6.35637084989848,9.3,5.63137084989848));
#13175=CARTESIAN_POINT('',(-6.35637084989848,8.9,5.63137084989848));
#13176=CARTESIAN_POINT('Origin',(-6.13137084989848,9.3,5.63137084989848));
#13177=CARTESIAN_POINT('Origin',(-3.86862915010152,8.9,5.63137084989848));
#13178=CARTESIAN_POINT('',(-4.09362915010152,9.,5.63137084989848));
#13179=CARTESIAN_POINT('Origin',(-3.86862915010152,9.,5.63137084989848));
#13180=CARTESIAN_POINT('',(-4.09362915010152,9.3,5.63137084989848));
#13181=CARTESIAN_POINT('',(-4.09362915010152,8.9,5.63137084989848));
#13182=CARTESIAN_POINT('Origin',(-3.86862915010152,9.3,5.63137084989848));
#13183=CARTESIAN_POINT('Origin',(-3.86862915010152,8.9,3.36862915010152));
#13184=CARTESIAN_POINT('',(-4.09362915010152,9.,3.36862915010152));
#13185=CARTESIAN_POINT('Origin',(-3.86862915010152,9.,3.36862915010152));
#13186=CARTESIAN_POINT('',(-4.09362915010152,9.3,3.36862915010152));
#13187=CARTESIAN_POINT('',(-4.09362915010152,8.9,3.36862915010152));
#13188=CARTESIAN_POINT('Origin',(-3.86862915010152,9.3,3.36862915010152));
#13189=CARTESIAN_POINT('Origin',(-5.,9.,4.5));
#13190=CARTESIAN_POINT('',(-5.62,9.3,4.5));
#13191=CARTESIAN_POINT('Origin',(-5.,9.3,4.5));
#13192=CARTESIAN_POINT('',(-5.62,9.,4.5));
#13193=CARTESIAN_POINT('',(-5.62,9.,4.5));
#13194=CARTESIAN_POINT('Origin',(-5.,9.,4.5));
#13195=CARTESIAN_POINT('Origin',(-5.,9.,4.5));
#13196=CARTESIAN_POINT('',(-7.,9.3,4.5));
#13197=CARTESIAN_POINT('Origin',(-5.,9.3,4.5));
#13198=CARTESIAN_POINT('',(-7.,9.,4.5));
#13199=CARTESIAN_POINT('',(-7.,9.,4.5));
#13200=CARTESIAN_POINT('Origin',(-5.,9.,4.5));
#13201=CARTESIAN_POINT('Origin',(-5.,9.3,4.5));
#13202=CARTESIAN_POINT('Origin',(-5.,9.,4.5));
#13203=CARTESIAN_POINT('',(0.,0.,0.));
#13204=CARTESIAN_POINT('Origin',(3.86862915010152,5.6,3.36862915010152));
#13205=CARTESIAN_POINT('',(3.64362915010152,5.7,3.36862915010152));
#13206=CARTESIAN_POINT('Origin',(3.86862915010152,5.7,3.36862915010152));
#13207=CARTESIAN_POINT('',(3.64362915010152,6.,3.36862915010152));
#13208=CARTESIAN_POINT('',(3.64362915010152,5.6,3.36862915010152));
#13209=CARTESIAN_POINT('Origin',(3.86862915010152,6.,3.36862915010152));
#13210=CARTESIAN_POINT('Origin',(3.86862915010152,5.6,5.63137084989848));
#13211=CARTESIAN_POINT('',(3.64362915010152,5.7,5.63137084989848));
#13212=CARTESIAN_POINT('Origin',(3.86862915010152,5.7,5.63137084989848));
#13213=CARTESIAN_POINT('',(3.64362915010152,6.,5.63137084989848));
#13214=CARTESIAN_POINT('',(3.64362915010152,5.6,5.63137084989848));
#13215=CARTESIAN_POINT('Origin',(3.86862915010152,6.,5.63137084989848));
#13216=CARTESIAN_POINT('Origin',(6.13137084989848,5.6,5.63137084989848));
#13217=CARTESIAN_POINT('',(5.90637084989848,5.7,5.63137084989848));
#13218=CARTESIAN_POINT('Origin',(6.13137084989848,5.7,5.63137084989848));
#13219=CARTESIAN_POINT('',(5.90637084989848,6.,5.63137084989848));
#13220=CARTESIAN_POINT('',(5.90637084989848,5.6,5.63137084989848));
#13221=CARTESIAN_POINT('Origin',(6.13137084989848,6.,5.63137084989848));
#13222=CARTESIAN_POINT('Origin',(6.13137084989848,5.6,3.36862915010152));
#13223=CARTESIAN_POINT('',(5.90637084989848,5.7,3.36862915010152));
#13224=CARTESIAN_POINT('Origin',(6.13137084989848,5.7,3.36862915010152));
#13225=CARTESIAN_POINT('',(5.90637084989848,6.,3.36862915010152));
#13226=CARTESIAN_POINT('',(5.90637084989848,5.6,3.36862915010152));
#13227=CARTESIAN_POINT('Origin',(6.13137084989848,6.,3.36862915010152));
#13228=CARTESIAN_POINT('Origin',(5.,5.7,4.5));
#13229=CARTESIAN_POINT('',(4.38,6.,4.5));
#13230=CARTESIAN_POINT('Origin',(5.,6.,4.5));
#13231=CARTESIAN_POINT('',(4.38,5.7,4.5));
#13232=CARTESIAN_POINT('',(4.38,5.7,4.5));
#13233=CARTESIAN_POINT('Origin',(5.,5.7,4.5));
#13234=CARTESIAN_POINT('Origin',(5.,5.7,4.5));
#13235=CARTESIAN_POINT('',(3.,6.,4.5));
#13236=CARTESIAN_POINT('Origin',(5.,6.,4.5));
#13237=CARTESIAN_POINT('',(3.,5.7,4.5));
#13238=CARTESIAN_POINT('',(3.,5.7,4.5));
#13239=CARTESIAN_POINT('Origin',(5.,5.7,4.5));
#13240=CARTESIAN_POINT('Origin',(5.,6.,4.5));
#13241=CARTESIAN_POINT('Origin',(5.,5.7,4.5));
#13242=CARTESIAN_POINT('',(0.,0.,0.));
#13243=CARTESIAN_POINT('Origin',(3.86862915010152,8.9,3.36862915010152));
#13244=CARTESIAN_POINT('',(3.64362915010152,9.,3.36862915010152));
#13245=CARTESIAN_POINT('Origin',(3.86862915010152,9.,3.36862915010152));
#13246=CARTESIAN_POINT('',(3.64362915010152,9.3,3.36862915010152));
#13247=CARTESIAN_POINT('',(3.64362915010152,8.9,3.36862915010152));
#13248=CARTESIAN_POINT('Origin',(3.86862915010152,9.3,3.36862915010152));
#13249=CARTESIAN_POINT('Origin',(3.86862915010152,8.9,5.63137084989848));
#13250=CARTESIAN_POINT('',(3.64362915010152,9.,5.63137084989848));
#13251=CARTESIAN_POINT('Origin',(3.86862915010152,9.,5.63137084989848));
#13252=CARTESIAN_POINT('',(3.64362915010152,9.3,5.63137084989848));
#13253=CARTESIAN_POINT('',(3.64362915010152,8.9,5.63137084989848));
#13254=CARTESIAN_POINT('Origin',(3.86862915010152,9.3,5.63137084989848));
#13255=CARTESIAN_POINT('Origin',(6.13137084989848,8.9,5.63137084989848));
#13256=CARTESIAN_POINT('',(5.90637084989848,9.,5.63137084989848));
#13257=CARTESIAN_POINT('Origin',(6.13137084989848,9.,5.63137084989848));
#13258=CARTESIAN_POINT('',(5.90637084989848,9.3,5.63137084989848));
#13259=CARTESIAN_POINT('',(5.90637084989848,8.9,5.63137084989848));
#13260=CARTESIAN_POINT('Origin',(6.13137084989848,9.3,5.63137084989848));
#13261=CARTESIAN_POINT('Origin',(6.13137084989848,8.9,3.36862915010152));
#13262=CARTESIAN_POINT('',(5.90637084989848,9.,3.36862915010152));
#13263=CARTESIAN_POINT('Origin',(6.13137084989848,9.,3.36862915010152));
#13264=CARTESIAN_POINT('',(5.90637084989848,9.3,3.36862915010152));
#13265=CARTESIAN_POINT('',(5.90637084989848,8.9,3.36862915010152));
#13266=CARTESIAN_POINT('Origin',(6.13137084989848,9.3,3.36862915010152));
#13267=CARTESIAN_POINT('Origin',(5.,9.,4.5));
#13268=CARTESIAN_POINT('',(4.38,9.3,4.5));
#13269=CARTESIAN_POINT('Origin',(5.,9.3,4.5));
#13270=CARTESIAN_POINT('',(4.38,9.,4.5));
#13271=CARTESIAN_POINT('',(4.38,9.,4.5));
#13272=CARTESIAN_POINT('Origin',(5.,9.,4.5));
#13273=CARTESIAN_POINT('Origin',(5.,9.,4.5));
#13274=CARTESIAN_POINT('',(3.,9.3,4.5));
#13275=CARTESIAN_POINT('Origin',(5.,9.3,4.5));
#13276=CARTESIAN_POINT('',(3.,9.,4.5));
#13277=CARTESIAN_POINT('',(3.,9.,4.5));
#13278=CARTESIAN_POINT('Origin',(5.,9.,4.5));
#13279=CARTESIAN_POINT('Origin',(5.,9.3,4.5));
#13280=CARTESIAN_POINT('Origin',(5.,9.,4.5));
#13281=CARTESIAN_POINT('',(0.,0.,0.));
#13282=CARTESIAN_POINT('',(0.,0.,0.));
#13283=CARTESIAN_POINT('Origin',(0.75,1.2,0.));
#13284=CARTESIAN_POINT('',(0.885663593019381,1.2,-0.16));
#13285=CARTESIAN_POINT('',(0.885663593019381,1.2,0.16));
#13286=CARTESIAN_POINT('Origin',(0.,1.2,0.));
#13287=CARTESIAN_POINT('',(0.93,1.2,-0.16));
#13288=CARTESIAN_POINT('',(0.93,1.2,-0.16));
#13289=CARTESIAN_POINT('',(0.93,1.2,0.16));
#13290=CARTESIAN_POINT('',(0.93,1.2,0.16));
#13291=CARTESIAN_POINT('',(0.57,1.2,0.16));
#13292=CARTESIAN_POINT('Origin',(0.57,0.,0.16));
#13293=CARTESIAN_POINT('',(0.885663593019381,-1.2,0.16));
#13294=CARTESIAN_POINT('',(0.885663593019381,0.,0.16));
#13295=CARTESIAN_POINT('',(0.93,-1.2,0.16));
#13296=CARTESIAN_POINT('',(0.93,0.,0.16));
#13297=CARTESIAN_POINT('',(0.57,-1.2,0.16));
#13298=CARTESIAN_POINT('Origin',(0.75,-1.2,0.));
#13299=CARTESIAN_POINT('',(0.885663593019381,-1.2,-0.16));
#13300=CARTESIAN_POINT('Origin',(0.,-1.2,0.));
#13301=CARTESIAN_POINT('',(0.93,-1.2,-0.16));
#13302=CARTESIAN_POINT('',(0.93,-1.2,0.16));
#13303=CARTESIAN_POINT('',(0.93,-1.2,-0.16));
#13304=CARTESIAN_POINT('Origin',(0.93,0.,-0.16));
#13305=CARTESIAN_POINT('',(0.885663593019381,0.,-0.16));
#13306=CARTESIAN_POINT('',(0.93,0.,-0.16));
#13307=CARTESIAN_POINT('Origin',(0.93,0.,0.16));
#13308=CARTESIAN_POINT('Origin',(1.05,1.5,0.));
#13309=CARTESIAN_POINT('',(-1.05,1.5,-1.28587913910472E-16));
#13310=CARTESIAN_POINT('Origin',(0.,1.5,0.));
#13311=CARTESIAN_POINT('',(-0.9,1.5,-1.10218211923262E-16));
#13312=CARTESIAN_POINT('Origin',(0.,1.5,0.));
#13313=CARTESIAN_POINT('Origin',(0.,1.315,0.));
#13314=CARTESIAN_POINT('',(-1.05,1.13,-1.28587913910472E-16));
#13315=CARTESIAN_POINT('Origin',(0.,1.13,0.));
#13316=CARTESIAN_POINT('',(-1.05,1.315,-1.28587913910472E-16));
#13317=CARTESIAN_POINT('Origin',(1.,1.13,0.));
#13318=CARTESIAN_POINT('',(-1.,1.13,-1.22464679914735E-16));
#13319=CARTESIAN_POINT('Origin',(0.,1.13,0.));
#13320=CARTESIAN_POINT('Origin',(0.,1.065,0.));
#13321=CARTESIAN_POINT('',(-1.,1.,-1.22464679914735E-16));
#13322=CARTESIAN_POINT('Origin',(0.,1.,0.));
#13323=CARTESIAN_POINT('',(-1.,1.065,-1.22464679914735E-16));
#13324=CARTESIAN_POINT('Origin',(1.05,1.,0.));
#13325=CARTESIAN_POINT('',(-1.05,1.,-1.28587913910472E-16));
#13326=CARTESIAN_POINT('Origin',(0.,1.,0.));
#13327=CARTESIAN_POINT('Origin',(0.,0.,0.));
#13328=CARTESIAN_POINT('',(-1.05,-1.,-1.28587913910472E-16));
#13329=CARTESIAN_POINT('Origin',(0.,-1.,0.));
#13330=CARTESIAN_POINT('',(-1.05,0.,-1.28587913910472E-16));
#13331=CARTESIAN_POINT('Origin',(1.,-1.,0.));
#13332=CARTESIAN_POINT('',(-1.,-1.,-1.22464679914735E-16));
#13333=CARTESIAN_POINT('Origin',(0.,-1.,0.));
#13334=CARTESIAN_POINT('Origin',(0.,-1.065,0.));
#13335=CARTESIAN_POINT('',(-1.,-1.13,-1.22464679914735E-16));
#13336=CARTESIAN_POINT('Origin',(0.,-1.13,0.));
#13337=CARTESIAN_POINT('',(-1.,-1.065,-1.22464679914735E-16));
#13338=CARTESIAN_POINT('Origin',(1.05,-1.13,0.));
#13339=CARTESIAN_POINT('',(-1.05,-1.13,-1.28587913910472E-16));
#13340=CARTESIAN_POINT('Origin',(0.,-1.13,0.));
#13341=CARTESIAN_POINT('Origin',(0.,-1.315,0.));
#13342=CARTESIAN_POINT('',(-1.05,-1.5,-1.28587913910472E-16));
#13343=CARTESIAN_POINT('Origin',(0.,-1.5,0.));
#13344=CARTESIAN_POINT('',(-1.05,-1.315,-1.28587913910472E-16));
#13345=CARTESIAN_POINT('Origin',(0.9,-1.5,0.));
#13346=CARTESIAN_POINT('',(-0.9,-1.5,-1.10218211923262E-16));
#13347=CARTESIAN_POINT('Origin',(0.,-1.5,0.));
#13348=CARTESIAN_POINT('Origin',(0.,0.,0.));
#13349=CARTESIAN_POINT('',(-0.9,0.,-1.10218211923262E-16));
#13350=CARTESIAN_POINT('',(0.,0.,0.));
#13351=CARTESIAN_POINT('Origin',(0.75,1.2,0.));
#13352=CARTESIAN_POINT('',(0.880582193778639,1.2,0.16));
#13353=CARTESIAN_POINT('',(0.880582193778639,1.2,-0.16));
#13354=CARTESIAN_POINT('Origin',(0.,1.2,0.));
#13355=CARTESIAN_POINT('',(0.583459510163302,1.2,0.16));
#13356=CARTESIAN_POINT('',(0.57,1.2,0.16));
#13357=CARTESIAN_POINT('',(0.583459510163302,1.2,-0.16));
#13358=CARTESIAN_POINT('Origin',(0.,1.2,0.));
#13359=CARTESIAN_POINT('',(0.93,1.2,-0.16));
#13360=CARTESIAN_POINT('Origin',(0.93,0.,-0.16));
#13361=CARTESIAN_POINT('',(0.880582193778639,-1.2,-0.16));
#13362=CARTESIAN_POINT('',(0.880582193778639,0.,-0.16));
#13363=CARTESIAN_POINT('',(0.583459510163302,-1.2,-0.16));
#13364=CARTESIAN_POINT('',(0.583459510163302,0.,-0.16));
#13365=CARTESIAN_POINT('',(0.93,-1.2,-0.16));
#13366=CARTESIAN_POINT('Origin',(0.75,-1.2,0.));
#13367=CARTESIAN_POINT('',(0.880582193778639,-1.2,0.16));
#13368=CARTESIAN_POINT('Origin',(0.,-1.2,0.));
#13369=CARTESIAN_POINT('',(0.583459510163302,-1.2,0.16));
#13370=CARTESIAN_POINT('Origin',(0.,-1.2,0.));
#13371=CARTESIAN_POINT('',(0.57,-1.2,0.16));
#13372=CARTESIAN_POINT('Origin',(0.57,0.,0.16));
#13373=CARTESIAN_POINT('',(0.880582193778639,0.,0.16));
#13374=CARTESIAN_POINT('',(0.583459510163302,0.,0.16));
#13375=CARTESIAN_POINT('Origin',(0.895,1.35,0.));
#13376=CARTESIAN_POINT('',(-0.895,1.35,-1.09605888523688E-16));
#13377=CARTESIAN_POINT('Origin',(0.,1.35,0.));
#13378=CARTESIAN_POINT('',(-0.605,1.35,-7.40911313484149E-17));
#13379=CARTESIAN_POINT('Origin',(0.,1.35,0.));
#13380=CARTESIAN_POINT('Origin',(0.,0.,0.));
#13381=CARTESIAN_POINT('',(-0.895,-1.35,-1.09605888523688E-16));
#13382=CARTESIAN_POINT('Origin',(0.,-1.35,0.));
#13383=CARTESIAN_POINT('',(-0.895,0.,-1.09605888523688E-16));
#13384=CARTESIAN_POINT('Origin',(0.605,-1.35,0.));
#13385=CARTESIAN_POINT('',(-0.605,-1.35,-7.40911313484149E-17));
#13386=CARTESIAN_POINT('Origin',(0.,-1.35,0.));
#13387=CARTESIAN_POINT('Origin',(0.,0.,0.));
#13388=CARTESIAN_POINT('',(-0.605,0.,-7.40911313484149E-17));
#13389=CARTESIAN_POINT('',(0.,0.,0.));
#13390=CARTESIAN_POINT('',(0.,0.,0.));
#13391=CARTESIAN_POINT('',(0.,0.,0.));
#13392=CARTESIAN_POINT('Origin',(0.0866025403784439,-0.4,-0.15));
#13393=CARTESIAN_POINT('',(0.173205080756888,-0.4,0.));
#13394=CARTESIAN_POINT('',(0.0866025403784439,-0.4,-0.15));
#13395=CARTESIAN_POINT('',(0.173205080756888,-0.4,0.));
#13396=CARTESIAN_POINT('',(0.0866025403784439,-0.64,-0.15));
#13397=CARTESIAN_POINT('',(0.0866025403784439,-0.4,-0.15));
#13398=CARTESIAN_POINT('',(0.173205080756888,-0.64,0.));
#13399=CARTESIAN_POINT('',(0.173205080756888,-0.64,0.));
#13400=CARTESIAN_POINT('',(0.173205080756888,-0.4,0.));
#13401=CARTESIAN_POINT('Origin',(-0.0866025403784438,-0.4,-0.15));
#13402=CARTESIAN_POINT('',(-0.0866025403784438,-0.4,-0.15));
#13403=CARTESIAN_POINT('',(0.0866025403784439,-0.4,-0.15));
#13404=CARTESIAN_POINT('',(-0.0866025403784438,-0.64,-0.15));
#13405=CARTESIAN_POINT('',(-0.0866025403784438,-0.4,-0.15));
#13406=CARTESIAN_POINT('',(0.0866025403784439,-0.64,-0.15));
#13407=CARTESIAN_POINT('Origin',(-0.173205080756888,-0.4,-2.77555756156289E-17));
#13408=CARTESIAN_POINT('',(-0.173205080756888,-0.4,-2.12115047744981E-17));
#13409=CARTESIAN_POINT('',(-0.0866025403784438,-0.4,-0.15));
#13410=CARTESIAN_POINT('',(-0.173205080756888,-0.64,-2.77555756156289E-17));
#13411=CARTESIAN_POINT('',(-0.173205080756888,-0.4,-2.12115047744981E-17));
#13412=CARTESIAN_POINT('',(-0.0866025403784438,-0.64,-0.15));
#13413=CARTESIAN_POINT('Origin',(-0.0866025403784439,-0.4,0.15));
#13414=CARTESIAN_POINT('',(-0.0866025403784439,-0.4,0.15));
#13415=CARTESIAN_POINT('',(-0.173205080756888,-0.4,-2.12115047744981E-17));
#13416=CARTESIAN_POINT('',(-0.0866025403784439,-0.64,0.15));
#13417=CARTESIAN_POINT('',(-0.0866025403784439,-0.4,0.15));
#13418=CARTESIAN_POINT('',(-0.173205080756888,-0.64,-2.12115047744981E-17));
#13419=CARTESIAN_POINT('Origin',(0.0866025403784439,-0.4,0.15));
#13420=CARTESIAN_POINT('',(0.0866025403784439,-0.4,0.15));
#13421=CARTESIAN_POINT('',(-0.0866025403784439,-0.4,0.15));
#13422=CARTESIAN_POINT('',(0.0866025403784439,-0.64,0.15));
#13423=CARTESIAN_POINT('',(0.0866025403784439,-0.4,0.15));
#13424=CARTESIAN_POINT('',(-0.0866025403784439,-0.64,0.15));
#13425=CARTESIAN_POINT('Origin',(0.173205080756888,-0.4,0.));
#13426=CARTESIAN_POINT('',(0.0866025403784439,-0.4,0.15));
#13427=CARTESIAN_POINT('',(0.0866025403784439,-0.64,0.15));
#13428=CARTESIAN_POINT('Origin',(0.,-0.4,-2.77555756156289E-17));
#13429=CARTESIAN_POINT('Origin',(0.,-0.64,-2.77555756156289E-17));
#13430=CARTESIAN_POINT('Origin',(0.,-1.,0.));
#13431=CARTESIAN_POINT('',(-0.1954,-1.,2.39295984553393E-17));
#13432=CARTESIAN_POINT('Origin',(0.,-1.,0.));
#13433=CARTESIAN_POINT('Origin',(0.3,0.4,0.));
#13434=CARTESIAN_POINT('',(-0.3,0.4,-3.67394039744206E-17));
#13435=CARTESIAN_POINT('Origin',(0.,0.4,0.));
#13436=CARTESIAN_POINT('Origin',(0.,0.375,0.));
#13437=CARTESIAN_POINT('',(-0.35,0.35,-4.28626379701573E-17));
#13438=CARTESIAN_POINT('Origin',(0.,0.35,0.));
#13439=CARTESIAN_POINT('',(-0.325,0.375,-3.9801020972289E-17));
#13440=CARTESIAN_POINT('Origin',(0.,0.19,0.));
#13441=CARTESIAN_POINT('',(-0.35,0.03,-4.28626379701574E-17));
#13442=CARTESIAN_POINT('Origin',(0.,0.03,0.));
#13443=CARTESIAN_POINT('',(-0.35,0.19,-4.28626379701574E-17));
#13444=CARTESIAN_POINT('Origin',(0.,0.0149999999999999,0.));
#13445=CARTESIAN_POINT('',(-0.32,-3.29597460435593E-17,-3.91886975727153E-17));
#13446=CARTESIAN_POINT('Origin',(0.,0.,0.));
#13447=CARTESIAN_POINT('',(-0.335,0.0149999999999999,-4.10256677714363E-17));
#13448=CARTESIAN_POINT('Origin',(0.22,0.,0.));
#13449=CARTESIAN_POINT('',(-0.22,-6.93889390390723E-18,-2.69422295812418E-17));
#13450=CARTESIAN_POINT('Origin',(0.,0.,0.));
#13451=CARTESIAN_POINT('Origin',(0.,-0.02,0.));
#13452=CARTESIAN_POINT('',(-0.1954,-0.0492,2.39295984553393E-17));
#13453=CARTESIAN_POINT('Origin',(0.,-0.0492,0.));
#13454=CARTESIAN_POINT('',(-0.21,-0.02,-2.57175827820944E-17));
#13455=CARTESIAN_POINT('Origin',(0.,-0.8,0.));
#13456=CARTESIAN_POINT('',(-0.1954,-0.8,-2.39295984553393E-17));
#13457=CARTESIAN_POINT('',(0.,0.,0.));
#13458=CARTESIAN_POINT('Origin',(0.115470053837925,-0.5,-0.2));
#13459=CARTESIAN_POINT('',(0.23094010767585,-0.5,0.));
#13460=CARTESIAN_POINT('',(0.115470053837925,-0.5,-0.2));
#13461=CARTESIAN_POINT('',(0.23094010767585,-0.5,0.));
#13462=CARTESIAN_POINT('',(0.115470053837925,-0.8,-0.2));
#13463=CARTESIAN_POINT('',(0.115470053837925,-0.5,-0.2));
#13464=CARTESIAN_POINT('',(0.23094010767585,-0.8,0.));
#13465=CARTESIAN_POINT('',(0.23094010767585,-0.8,0.));
#13466=CARTESIAN_POINT('',(0.23094010767585,-0.5,0.));
#13467=CARTESIAN_POINT('Origin',(-0.115470053837925,-0.5,-0.2));
#13468=CARTESIAN_POINT('',(-0.115470053837925,-0.5,-0.2));
#13469=CARTESIAN_POINT('',(0.115470053837925,-0.5,-0.2));
#13470=CARTESIAN_POINT('',(-0.115470053837925,-0.8,-0.2));
#13471=CARTESIAN_POINT('',(-0.115470053837925,-0.5,-0.2));
#13472=CARTESIAN_POINT('',(0.115470053837925,-0.8,-0.2));
#13473=CARTESIAN_POINT('Origin',(-0.23094010767585,-0.5,-2.77555756156289E-17));
#13474=CARTESIAN_POINT('',(-0.23094010767585,-0.5,-2.82820063659975E-17));
#13475=CARTESIAN_POINT('',(-0.115470053837925,-0.5,-0.2));
#13476=CARTESIAN_POINT('',(-0.23094010767585,-0.8,-2.77555756156289E-17));
#13477=CARTESIAN_POINT('',(-0.23094010767585,-0.5,-2.82820063659975E-17));
#13478=CARTESIAN_POINT('',(-0.115470053837925,-0.8,-0.2));
#13479=CARTESIAN_POINT('Origin',(-0.115470053837925,-0.5,0.2));
#13480=CARTESIAN_POINT('',(-0.115470053837925,-0.5,0.2));
#13481=CARTESIAN_POINT('',(-0.23094010767585,-0.5,-2.82820063659975E-17));
#13482=CARTESIAN_POINT('',(-0.115470053837925,-0.8,0.2));
#13483=CARTESIAN_POINT('',(-0.115470053837925,-0.5,0.2));
#13484=CARTESIAN_POINT('',(-0.23094010767585,-0.8,-2.82820063659975E-17));
#13485=CARTESIAN_POINT('Origin',(0.115470053837925,-0.5,0.2));
#13486=CARTESIAN_POINT('',(0.115470053837925,-0.5,0.2));
#13487=CARTESIAN_POINT('',(-0.115470053837925,-0.5,0.2));
#13488=CARTESIAN_POINT('',(0.115470053837925,-0.8,0.2));
#13489=CARTESIAN_POINT('',(0.115470053837925,-0.5,0.2));
#13490=CARTESIAN_POINT('',(-0.115470053837925,-0.8,0.2));
#13491=CARTESIAN_POINT('Origin',(0.23094010767585,-0.5,0.));
#13492=CARTESIAN_POINT('',(0.115470053837925,-0.5,0.2));
#13493=CARTESIAN_POINT('',(0.115470053837925,-0.8,0.2));
#13494=CARTESIAN_POINT('Origin',(0.,-0.5,0.));
#13495=CARTESIAN_POINT('Origin',(0.,-0.8,0.));
#13496=CARTESIAN_POINT('Origin',(0.,-1.99,0.));
#13497=CARTESIAN_POINT('',(-0.25,-1.99,3.06161699786838E-17));
#13498=CARTESIAN_POINT('Origin',(0.,-1.99,0.));
#13499=CARTESIAN_POINT('',(-0.21,-1.99,2.57175827820944E-17));
#13500=CARTESIAN_POINT('Origin',(0.,-1.99,0.));
#13501=CARTESIAN_POINT('Origin',(0.,-2.2,0.));
#13502=CARTESIAN_POINT('',(-0.25,-2.2,3.06161699786838E-17));
#13503=CARTESIAN_POINT('',(-0.25,-2.2,3.06161699786838E-17));
#13504=CARTESIAN_POINT('Origin',(0.,-2.2,0.));
#13505=CARTESIAN_POINT('Origin',(0.,-2.2,0.));
#13506=CARTESIAN_POINT('Origin',(0.375,0.5,0.));
#13507=CARTESIAN_POINT('',(-0.375,0.5,-4.59242549680257E-17));
#13508=CARTESIAN_POINT('Origin',(0.,0.5,0.));
#13509=CARTESIAN_POINT('Origin',(0.,0.475,0.));
#13510=CARTESIAN_POINT('',(-0.425,0.45,-5.20474889637625E-17));
#13511=CARTESIAN_POINT('Origin',(0.,0.45,0.));
#13512=CARTESIAN_POINT('',(-0.4,0.475,-4.89858719658941E-17));
#13513=CARTESIAN_POINT('Origin',(0.,0.24,0.));
#13514=CARTESIAN_POINT('',(-0.425,0.0299999999999998,-5.20474889637625E-17));
#13515=CARTESIAN_POINT('Origin',(0.,0.0299999999999998,0.));
#13516=CARTESIAN_POINT('',(-0.425,0.24,-5.20474889637625E-17));
#13517=CARTESIAN_POINT('Origin',(0.,0.0150000000000001,0.));
#13518=CARTESIAN_POINT('',(-0.395,4.85722573273506E-17,-4.83735485663204E-17));
#13519=CARTESIAN_POINT('Origin',(0.,0.,0.));
#13520=CARTESIAN_POINT('',(-0.41,0.0150000000000001,-5.02105187650415E-17));
#13521=CARTESIAN_POINT('Origin',(0.27,0.,0.));
#13522=CARTESIAN_POINT('',(-0.27,0.,-3.30654635769785E-17));
#13523=CARTESIAN_POINT('Origin',(0.,0.,0.));
#13524=CARTESIAN_POINT('Origin',(0.,-0.02,0.));
#13525=CARTESIAN_POINT('',(-0.24505,-0.0498999999999999,3.00099698131059E-17));
#13526=CARTESIAN_POINT('Origin',(0.,-0.0498999999999999,0.));
#13527=CARTESIAN_POINT('',(-0.26,-0.02,-3.18408167778312E-17));
#13528=CARTESIAN_POINT('Origin',(0.,-0.995,0.));
#13529=CARTESIAN_POINT('',(-0.24505,-1.95495,3.00099698131059E-17));
#13530=CARTESIAN_POINT('Origin',(0.,-1.95495,0.));
#13531=CARTESIAN_POINT('',(-0.24505,-0.995,-3.00099698131059E-17));
#13532=CARTESIAN_POINT('Origin',(0.,-1.975,0.));
#13533=CARTESIAN_POINT('',(-0.225,-1.975,-2.75545529808154E-17));
#13534=CARTESIAN_POINT('',(0.,0.,0.));
#13535=CARTESIAN_POINT('',(0.,0.,0.));
#13536=CARTESIAN_POINT('',(0.,0.,0.));
#13537=CARTESIAN_POINT('',(0.,0.,0.));
#13538=CARTESIAN_POINT('',(0.,0.,0.));
#13539=CARTESIAN_POINT('',(0.,0.,0.));
#13540=CARTESIAN_POINT('',(0.,0.,0.));
#13541=CARTESIAN_POINT('',(0.,0.,0.));
#13542=CARTESIAN_POINT('',(0.,0.,0.));
#13543=CARTESIAN_POINT('',(0.,0.,0.));
#13544=CARTESIAN_POINT('',(-1.2,0.6,0.8));
#13545=CARTESIAN_POINT('',(1.2,0.6,0.8));
#13546=CARTESIAN_POINT('',(1.,0.8,8.5));
#13547=CARTESIAN_POINT('',(0.,0.8,9.3));
#13548=CARTESIAN_POINT('',(0.,12.6,0.));
#13549=CARTESIAN_POINT('',(-1.2,12.,0.8));
#13550=CARTESIAN_POINT('',(1.2,12.,0.8));
#13551=CARTESIAN_POINT('',(1.,11.8,8.5));
#13552=CARTESIAN_POINT('',(0.,11.8,9.3));
#13553=CARTESIAN_POINT('',(0.,0.,0.));
#13554=CARTESIAN_POINT('',(0.,0.,0.));
#13555=CARTESIAN_POINT('',(0.,0.,0.));
#13556=CARTESIAN_POINT('',(-2.,0.,2.5));
#13557=CARTESIAN_POINT('',(-2.,-0.57,2.5));
#13558=CARTESIAN_POINT('',(-2.,12.6,2.5));
#13559=CARTESIAN_POINT('',(-2.,12.7,2.5));
#13560=CARTESIAN_POINT('',(0.,0.,4.));
#13561=CARTESIAN_POINT('',(-2.,0.,6.5));
#13562=CARTESIAN_POINT('',(-2.,-0.57,6.5));
#13563=CARTESIAN_POINT('',(-2.,12.6,6.5));
#13564=CARTESIAN_POINT('',(-2.,12.7,6.5));
#13565=CARTESIAN_POINT('',(4.,0.,0.));
#13566=CARTESIAN_POINT('',(2.,0.,2.5));
#13567=CARTESIAN_POINT('',(2.,-0.57,2.5));
#13568=CARTESIAN_POINT('',(2.,12.6,2.5));
#13569=CARTESIAN_POINT('',(2.,12.7,2.5));
#13570=CARTESIAN_POINT('',(4.,0.,4.));
#13571=CARTESIAN_POINT('',(2.,0.,6.5));
#13572=CARTESIAN_POINT('',(2.,-0.57,6.5));
#13573=CARTESIAN_POINT('',(2.,12.6,6.5));
#13574=CARTESIAN_POINT('',(2.,12.7,6.5));
#13575=CARTESIAN_POINT('',(0.,0.,0.));
#13576=CARTESIAN_POINT('',(0.,0.,0.));
#13577=CARTESIAN_POINT('',(0.,0.,0.));
#13578=CARTESIAN_POINT('',(0.,0.,0.));
#13579=CARTESIAN_POINT('',(0.,0.,0.));
#13580=CARTESIAN_POINT('',(-5.,7.5,4.5));
#13581=CARTESIAN_POINT('',(-3.86862915010152,5.7,5.63137084989848));
#13582=CARTESIAN_POINT('',(-6.13137084989848,5.7,5.63137084989848));
#13583=CARTESIAN_POINT('',(-6.13137084989848,5.7,3.36862915010152));
#13584=CARTESIAN_POINT('',(-3.86862915010152,5.7,3.36862915010152));
#13585=CARTESIAN_POINT('',(-3.86862915010152,9.3,5.63137084989848));
#13586=CARTESIAN_POINT('',(-6.13137084989848,9.3,5.63137084989848));
#13587=CARTESIAN_POINT('',(-6.13137084989848,9.3,3.36862915010152));
#13588=CARTESIAN_POINT('',(-3.86862915010152,9.3,3.36862915010152));
#13589=CARTESIAN_POINT('',(5.,7.5,4.5));
#13590=CARTESIAN_POINT('',(6.13137084989848,5.7,5.63137084989848));
#13591=CARTESIAN_POINT('',(3.86862915010152,5.7,5.63137084989848));
#13592=CARTESIAN_POINT('',(3.86862915010152,5.7,3.36862915010152));
#13593=CARTESIAN_POINT('',(6.13137084989848,5.7,3.36862915010152));
#13594=CARTESIAN_POINT('',(6.13137084989848,9.3,5.63137084989848));
#13595=CARTESIAN_POINT('',(3.86862915010152,9.3,5.63137084989848));
#13596=CARTESIAN_POINT('',(3.86862915010152,9.3,3.36862915010152));
#13597=CARTESIAN_POINT('',(6.13137084989848,9.3,3.36862915010152));
#13598=CARTESIAN_POINT('',(-2.9,0.9,1.4));
#13599=CARTESIAN_POINT('',(-2.9,11.7,1.4));
#13600=CARTESIAN_POINT('',(2.9,0.9,1.4));
#13601=CARTESIAN_POINT('',(2.9,11.7,1.4));
#13602=CARTESIAN_POINT('',(0.,0.,0.));
#13603=CARTESIAN_POINT('',(0.,0.,0.));
#13604=CARTESIAN_POINT('Origin',(0.,3.2,4.5));
#13605=CARTESIAN_POINT('',(-0.4,3.2,4.5));
#13606=CARTESIAN_POINT('Origin',(0.,3.2,4.5));
#13607=CARTESIAN_POINT('',(-0.4,3.6,4.5));
#13608=CARTESIAN_POINT('',(-0.4,3.2,4.5));
#13609=CARTESIAN_POINT('Origin',(0.,3.6,4.5));
#13610=CARTESIAN_POINT('Origin',(0.,3.2,4.5));
#13611=CARTESIAN_POINT('',(-0.225,3.2,4.5));
#13612=CARTESIAN_POINT('Origin',(0.,3.2,4.5));
#13613=CARTESIAN_POINT('Origin',(0.,2.8,4.5));
#13614=CARTESIAN_POINT('',(-0.9,2.8,4.5));
#13615=CARTESIAN_POINT('Origin',(0.,2.8,4.5));
#13616=CARTESIAN_POINT('',(-0.9,3.1,4.5));
#13617=CARTESIAN_POINT('',(-0.9,2.8,4.5));
#13618=CARTESIAN_POINT('Origin',(0.,3.1,4.5));
#13619=CARTESIAN_POINT('Origin',(0.,3.1,4.5));
#13620=CARTESIAN_POINT('',(-0.99,3.1,4.5));
#13621=CARTESIAN_POINT('Origin',(0.,3.1,4.5));
#13622=CARTESIAN_POINT('Origin',(0.,2.8,4.5));
#13623=CARTESIAN_POINT('',(-0.99,2.8,4.5));
#13624=CARTESIAN_POINT('Origin',(0.,2.8,4.5));
#13625=CARTESIAN_POINT('Origin',(0.,2.4,4.5));
#13626=CARTESIAN_POINT('',(-0.99,2.4,4.5));
#13627=CARTESIAN_POINT('',(-0.99,2.4,4.5));
#13628=CARTESIAN_POINT('Origin',(0.,2.4,4.5));
#13629=CARTESIAN_POINT('Origin',(0.,2.4,4.5));
#13630=CARTESIAN_POINT('',(-0.225,2.4,4.5));
#13631=CARTESIAN_POINT('',(-0.225,2.4,4.5));
#13632=CARTESIAN_POINT('Origin',(0.,2.4,4.5));
#13633=CARTESIAN_POINT('Origin',(0.,2.4,4.5));
#13634=CARTESIAN_POINT('',(-0.99,3.6,4.5));
#13635=CARTESIAN_POINT('Origin',(0.,3.6,4.5));
#13636=CARTESIAN_POINT('',(-0.99,2.4,4.5));
#13637=CARTESIAN_POINT('Origin',(0.,3.6,4.5));
#13638=CARTESIAN_POINT('Origin',(0.,2.4,4.5));
#13639=CARTESIAN_POINT('',(0.,0.,0.));
#13640=CARTESIAN_POINT('Origin',(0.,2.95,4.5));
#13641=CARTESIAN_POINT('',(-1.10218211923262E-16,2.95,5.4));
#13642=CARTESIAN_POINT('Origin',(-1.16341445918999E-16,2.95,5.45));
#13643=CARTESIAN_POINT('Origin',(0.,2.95,4.5));
#13644=CARTESIAN_POINT('',(0.,0.,0.));
#13645=CARTESIAN_POINT('Origin',(0.,1.2,4.5));
#13646=CARTESIAN_POINT('',(-0.165,1.2,4.5));
#13647=CARTESIAN_POINT('Origin',(0.,1.2,4.5));
#13648=CARTESIAN_POINT('',(-0.165,2.4,4.5));
#13649=CARTESIAN_POINT('',(-0.165,1.2,4.5));
#13650=CARTESIAN_POINT('Origin',(0.,2.4,4.5));
#13651=CARTESIAN_POINT('Origin',(0.,1.2,4.5));
#13652=CARTESIAN_POINT('Origin',(0.,-5.6,4.5));
#13653=CARTESIAN_POINT('',(-0.4,2.4,4.5));
#13654=CARTESIAN_POINT('Origin',(0.,2.4,4.5));
#13655=CARTESIAN_POINT('',(-0.4,-5.6,4.5));
#13656=CARTESIAN_POINT('',(-0.4,-5.6,4.5));
#13657=CARTESIAN_POINT('Origin',(0.,-5.6,4.5));
#13658=CARTESIAN_POINT('Origin',(0.,2.4,4.5));
#13659=CARTESIAN_POINT('Origin',(0.,-5.6,4.5));
#13660=CARTESIAN_POINT('',(0.,0.,0.));
#13661=CARTESIAN_POINT('Origin',(0.3,0.4,0.));
#13662=CARTESIAN_POINT('',(-0.3,0.4,-3.67394039744206E-17));
#13663=CARTESIAN_POINT('Origin',(0.,0.4,0.));
#13664=CARTESIAN_POINT('Origin',(0.,0.375,0.));
#13665=CARTESIAN_POINT('',(-0.35,0.35,-4.28626379701573E-17));
#13666=CARTESIAN_POINT('Origin',(0.,0.35,0.));
#13667=CARTESIAN_POINT('',(-0.325,0.375,-3.9801020972289E-17));
#13668=CARTESIAN_POINT('Origin',(0.,0.19,0.));
#13669=CARTESIAN_POINT('',(-0.35,0.03,-4.28626379701574E-17));
#13670=CARTESIAN_POINT('Origin',(0.,0.03,0.));
#13671=CARTESIAN_POINT('',(-0.35,0.19,-4.28626379701574E-17));
#13672=CARTESIAN_POINT('Origin',(0.,0.0149999999999999,0.));
#13673=CARTESIAN_POINT('',(-0.32,-3.29597460435593E-17,-3.91886975727153E-17));
#13674=CARTESIAN_POINT('Origin',(0.,0.,0.));
#13675=CARTESIAN_POINT('',(-0.335,0.0149999999999999,-4.10256677714363E-17));
#13676=CARTESIAN_POINT('Origin',(0.22,0.,0.));
#13677=CARTESIAN_POINT('',(-0.22,-6.93889390390723E-18,-2.69422295812418E-17));
#13678=CARTESIAN_POINT('Origin',(0.,0.,0.));
#13679=CARTESIAN_POINT('Origin',(0.,-0.02,0.));
#13680=CARTESIAN_POINT('',(-0.1954,-0.0492,2.39295984553393E-17));
#13681=CARTESIAN_POINT('Origin',(0.,-0.0492,0.));
#13682=CARTESIAN_POINT('',(-0.21,-0.02,-2.57175827820944E-17));
#13683=CARTESIAN_POINT('Origin',(0.,-0.8,0.));
#13684=CARTESIAN_POINT('',(-0.1954,-1.5646,2.39295984553393E-17));
#13685=CARTESIAN_POINT('Origin',(0.,-1.5646,0.));
#13686=CARTESIAN_POINT('',(-0.1954,-0.8,-2.39295984553393E-17));
#13687=CARTESIAN_POINT('Origin',(0.,-1.58,0.));
#13688=CARTESIAN_POINT('',(-0.16,-1.6,-1.95943487863577E-17));
#13689=CARTESIAN_POINT('Origin',(0.,-1.6,0.));
#13690=CARTESIAN_POINT('',(-0.18,-1.58,-2.20436423846524E-17));
#13691=CARTESIAN_POINT('Origin',(0.,-1.6,0.));
#13692=CARTESIAN_POINT('Origin',(0.0866025403784439,-0.4,-0.15));
#13693=CARTESIAN_POINT('',(0.173205080756888,-0.4,0.));
#13694=CARTESIAN_POINT('',(0.0866025403784439,-0.4,-0.15));
#13695=CARTESIAN_POINT('',(0.173205080756888,-0.4,0.));
#13696=CARTESIAN_POINT('',(0.0866025403784439,-0.64,-0.15));
#13697=CARTESIAN_POINT('',(0.0866025403784439,-0.4,-0.15));
#13698=CARTESIAN_POINT('',(0.173205080756888,-0.64,0.));
#13699=CARTESIAN_POINT('',(0.173205080756888,-0.64,0.));
#13700=CARTESIAN_POINT('',(0.173205080756888,-0.4,0.));
#13701=CARTESIAN_POINT('Origin',(-0.0866025403784438,-0.4,-0.15));
#13702=CARTESIAN_POINT('',(-0.0866025403784438,-0.4,-0.15));
#13703=CARTESIAN_POINT('',(0.0866025403784439,-0.4,-0.15));
#13704=CARTESIAN_POINT('',(-0.0866025403784438,-0.64,-0.15));
#13705=CARTESIAN_POINT('',(-0.0866025403784438,-0.4,-0.15));
#13706=CARTESIAN_POINT('',(0.0866025403784439,-0.64,-0.15));
#13707=CARTESIAN_POINT('Origin',(-0.173205080756888,-0.4,-2.77555756156289E-17));
#13708=CARTESIAN_POINT('',(-0.173205080756888,-0.4,-2.12115047744981E-17));
#13709=CARTESIAN_POINT('',(-0.0866025403784438,-0.4,-0.15));
#13710=CARTESIAN_POINT('',(-0.173205080756888,-0.64,-2.77555756156289E-17));
#13711=CARTESIAN_POINT('',(-0.173205080756888,-0.4,-2.12115047744981E-17));
#13712=CARTESIAN_POINT('',(-0.0866025403784438,-0.64,-0.15));
#13713=CARTESIAN_POINT('Origin',(-0.0866025403784439,-0.4,0.15));
#13714=CARTESIAN_POINT('',(-0.0866025403784439,-0.4,0.15));
#13715=CARTESIAN_POINT('',(-0.173205080756888,-0.4,-2.12115047744981E-17));
#13716=CARTESIAN_POINT('',(-0.0866025403784439,-0.64,0.15));
#13717=CARTESIAN_POINT('',(-0.0866025403784439,-0.4,0.15));
#13718=CARTESIAN_POINT('',(-0.173205080756888,-0.64,-2.12115047744981E-17));
#13719=CARTESIAN_POINT('Origin',(0.0866025403784439,-0.4,0.15));
#13720=CARTESIAN_POINT('',(0.0866025403784439,-0.4,0.15));
#13721=CARTESIAN_POINT('',(-0.0866025403784439,-0.4,0.15));
#13722=CARTESIAN_POINT('',(0.0866025403784439,-0.64,0.15));
#13723=CARTESIAN_POINT('',(0.0866025403784439,-0.4,0.15));
#13724=CARTESIAN_POINT('',(-0.0866025403784439,-0.64,0.15));
#13725=CARTESIAN_POINT('Origin',(0.173205080756888,-0.4,0.));
#13726=CARTESIAN_POINT('',(0.0866025403784439,-0.4,0.15));
#13727=CARTESIAN_POINT('',(0.0866025403784439,-0.64,0.15));
#13728=CARTESIAN_POINT('Origin',(0.,-0.4,-2.77555756156289E-17));
#13729=CARTESIAN_POINT('Origin',(0.,-0.64,-2.77555756156289E-17));
#13730=CARTESIAN_POINT('',(0.,0.,0.));
#13731=CARTESIAN_POINT('Origin',(-1.1,-6.1,4.5));
#13732=CARTESIAN_POINT('',(-1.,-6.1,4.805));
#13733=CARTESIAN_POINT('Origin',(-1.,-6.1,4.5));
#13734=CARTESIAN_POINT('',(-0.5,-6.1,4.805));
#13735=CARTESIAN_POINT('',(-1.1,-6.1,4.805));
#13736=CARTESIAN_POINT('Origin',(-0.5,-6.1,4.5));
#13737=CARTESIAN_POINT('Origin',(-1.1,-6.1,4.5));
#13738=CARTESIAN_POINT('',(0.5,-6.1,4.805));
#13739=CARTESIAN_POINT('Origin',(0.5,-6.1,4.5));
#13740=CARTESIAN_POINT('',(1.,-6.1,4.805));
#13741=CARTESIAN_POINT('',(-1.1,-6.1,4.805));
#13742=CARTESIAN_POINT('Origin',(1.,-6.1,4.5));
#13743=CARTESIAN_POINT('Origin',(0.,-5.3,4.89));
#13744=CARTESIAN_POINT('',(0.0888819441731535,-5.43901438774458,4.89));
#13745=CARTESIAN_POINT('',(0.0888819441731535,-5.16098561225542,4.89));
#13746=CARTESIAN_POINT('',(0.0888819441731535,-5.6,4.89));
#13747=CARTESIAN_POINT('Origin',(0.,-5.3,4.89));
#13748=CARTESIAN_POINT('Origin',(0.,-5.3,4.89));
#13749=CARTESIAN_POINT('',(-0.0888819441731535,-5.43901438774458,4.89));
#13750=CARTESIAN_POINT('Ctrl Pts',(-0.0888819441731541,-5.43901438774458,
4.89));
#13751=CARTESIAN_POINT('Ctrl Pts',(-0.0808964434200148,-5.44412009546053,
4.89181991495419));
#13752=CARTESIAN_POINT('Ctrl Pts',(-0.0723643333023662,-5.44859639186021,
4.89350251788328));
#13753=CARTESIAN_POINT('Ctrl Pts',(-0.0431949313468613,-5.46075622416973,
4.89819171553211));
#13754=CARTESIAN_POINT('Ctrl Pts',(-0.0209808024963256,-5.465,4.9));
#13755=CARTESIAN_POINT('Ctrl Pts',(0.0209808024963256,-5.465,4.9));
#13756=CARTESIAN_POINT('Ctrl Pts',(0.0431949313468613,-5.46075622416973,
4.89819171553211));
#13757=CARTESIAN_POINT('Ctrl Pts',(0.0723643333023662,-5.44859639186021,
4.89350251788328));
#13758=CARTESIAN_POINT('Ctrl Pts',(0.0808964434200144,-5.44412009546053,
4.89181991495419));
#13759=CARTESIAN_POINT('Ctrl Pts',(0.0888819441731541,-5.43901438774458,
4.89));
#13760=CARTESIAN_POINT('',(-0.165,-5.3,4.89));
#13761=CARTESIAN_POINT('Origin',(0.,-5.3,4.89));
#13762=CARTESIAN_POINT('',(-0.165,-5.3,5.5));
#13763=CARTESIAN_POINT('',(-0.165,-5.3,4.89));
#13764=CARTESIAN_POINT('Origin',(0.,-5.3,5.5));
#13765=CARTESIAN_POINT('',(-0.0888819441731535,-5.16098561225542,4.89));
#13766=CARTESIAN_POINT('Origin',(0.,-5.3,4.89));
#13767=CARTESIAN_POINT('Ctrl Pts',(0.0888819441731536,-5.16098561225542,
4.89));
#13768=CARTESIAN_POINT('Ctrl Pts',(0.0808964434200141,-5.15587990453947,
4.89181991495419));
#13769=CARTESIAN_POINT('Ctrl Pts',(0.0723643333023662,-5.15140360813979,
4.89350251788328));
#13770=CARTESIAN_POINT('Ctrl Pts',(0.0431949313468613,-5.13924377583027,
4.89819171553211));
#13771=CARTESIAN_POINT('Ctrl Pts',(0.0209808024963256,-5.135,4.9));
#13772=CARTESIAN_POINT('Ctrl Pts',(-0.0209808024963256,-5.135,4.9));
#13773=CARTESIAN_POINT('Ctrl Pts',(-0.0431949313468613,-5.13924377583027,
4.89819171553211));
#13774=CARTESIAN_POINT('Ctrl Pts',(-0.0723643333023663,-5.15140360813979,
4.89350251788328));
#13775=CARTESIAN_POINT('Ctrl Pts',(-0.0808964434200144,-5.15587990453947,
4.89181991495419));
#13776=CARTESIAN_POINT('Ctrl Pts',(-0.0888819441731536,-5.16098561225542,
4.89));
#13777=CARTESIAN_POINT('Origin',(0.,-5.3,4.89));
#13778=CARTESIAN_POINT('',(-0.0888819441731535,-5.6,4.89));
#13779=CARTESIAN_POINT('Origin',(0.,-5.6,4.5));
#13780=CARTESIAN_POINT('',(-0.4,-5.6,4.5));
#13781=CARTESIAN_POINT('Origin',(0.,-5.6,4.5));
#13782=CARTESIAN_POINT('',(-0.4,-5.,4.5));
#13783=CARTESIAN_POINT('',(-0.4,-5.6,4.5));
#13784=CARTESIAN_POINT('Origin',(0.,-5.,4.5));
#13785=CARTESIAN_POINT('Origin',(0.5,-6.7,3.4));
#13786=CARTESIAN_POINT('',(0.5,-5.6,5.5));
#13787=CARTESIAN_POINT('',(0.5,-6.6,5.5));
#13788=CARTESIAN_POINT('',(0.5,-6.25,5.5));
#13789=CARTESIAN_POINT('',(0.5,-5.6,3.5));
#13790=CARTESIAN_POINT('',(0.5,-5.6,3.4));
#13791=CARTESIAN_POINT('',(0.5,-6.6,3.5));
#13792=CARTESIAN_POINT('',(0.5,-6.25,3.5));
#13793=CARTESIAN_POINT('',(0.5,-6.6,3.45));
#13794=CARTESIAN_POINT('Origin',(0.5,-5.6,3.4));
#13795=CARTESIAN_POINT('',(-0.5,-5.6,5.5));
#13796=CARTESIAN_POINT('',(0.25,-5.6,5.5));
#13797=CARTESIAN_POINT('',(-0.5,-5.6,3.5));
#13798=CARTESIAN_POINT('',(-0.5,-5.6,3.4));
#13799=CARTESIAN_POINT('',(0.25,-5.6,3.5));
#13800=CARTESIAN_POINT('Origin',(-0.5,-5.6,3.4));
#13801=CARTESIAN_POINT('',(-0.5,-6.6,5.5));
#13802=CARTESIAN_POINT('',(-0.5,-5.7,5.5));
#13803=CARTESIAN_POINT('',(-0.5,-6.6,3.5));
#13804=CARTESIAN_POINT('',(-0.5,-6.6,3.45));
#13805=CARTESIAN_POINT('',(-0.5,-5.7,3.5));
#13806=CARTESIAN_POINT('Origin',(0.,-5.8,3.5));
#13807=CARTESIAN_POINT('',(-1.,-6.6,3.5));
#13808=CARTESIAN_POINT('',(-1.,-6.6,3.5));
#13809=CARTESIAN_POINT('',(-1.,-5.,3.5));
#13810=CARTESIAN_POINT('',(-1.,-5.,3.5));
#13811=CARTESIAN_POINT('',(1.,-5.,3.5));
#13812=CARTESIAN_POINT('',(1.,-5.,3.5));
#13813=CARTESIAN_POINT('',(1.,-6.6,3.5));
#13814=CARTESIAN_POINT('',(1.,-6.6,3.5));
#13815=CARTESIAN_POINT('',(-1.,-6.6,3.5));
#13816=CARTESIAN_POINT('Origin',(-1.,-6.6,3.5));
#13817=CARTESIAN_POINT('',(-1.,-6.6,5.5));
#13818=CARTESIAN_POINT('',(-1.,-6.6,5.5));
#13819=CARTESIAN_POINT('',(-1.,-6.6,3.5));
#13820=CARTESIAN_POINT('Origin',(-1.,-6.6,3.5));
#13821=CARTESIAN_POINT('',(1.,-6.6,5.5));
#13822=CARTESIAN_POINT('',(1.,-6.6,3.5));
#13823=CARTESIAN_POINT('',(-1.,-6.6,5.5));
#13824=CARTESIAN_POINT('Origin',(1.,-5.,3.5));
#13825=CARTESIAN_POINT('',(-1.,-5.,5.5));
#13826=CARTESIAN_POINT('',(-1.,-5.,3.5));
#13827=CARTESIAN_POINT('',(1.,-5.,5.5));
#13828=CARTESIAN_POINT('',(1.,-5.,5.5));
#13829=CARTESIAN_POINT('',(1.,-5.,3.5));
#13830=CARTESIAN_POINT('Origin',(1.,-6.6,3.5));
#13831=CARTESIAN_POINT('',(1.,-6.6,5.5));
#13832=CARTESIAN_POINT('Origin',(-1.,-5.,3.5));
#13833=CARTESIAN_POINT('',(-1.,-5.,5.5));
#13834=CARTESIAN_POINT('Origin',(0.,-5.8,5.5));
#13835=CARTESIAN_POINT('',(0.,0.,0.));
#13836=CARTESIAN_POINT('Origin',(0.0577350269189626,0.,-0.1));
#13837=CARTESIAN_POINT('',(0.0577350269189626,0.,-0.1));
#13838=CARTESIAN_POINT('',(0.115470053837925,0.,0.));
#13839=CARTESIAN_POINT('',(0.0934187836487032,0.,-0.0381939203391614));
#13840=CARTESIAN_POINT('',(0.0577350269189626,-0.2,-0.1));
#13841=CARTESIAN_POINT('',(0.0577350269189626,0.,-0.1));
#13842=CARTESIAN_POINT('',(0.115470053837925,-0.2,0.));
#13843=CARTESIAN_POINT('',(0.115470053837925,-0.2,0.));
#13844=CARTESIAN_POINT('',(0.115470053837925,0.,0.));
#13845=CARTESIAN_POINT('Origin',(-0.0577350269189626,0.,-0.1));
#13846=CARTESIAN_POINT('',(-0.0577350269189626,0.,-0.1));
#13847=CARTESIAN_POINT('',(0.0561324865405187,0.,-0.1));
#13848=CARTESIAN_POINT('',(-0.0577350269189626,-0.2,-0.1));
#13849=CARTESIAN_POINT('',(-0.0577350269189626,0.,-0.1));
#13850=CARTESIAN_POINT('',(0.0577350269189626,-0.2,-0.1));
#13851=CARTESIAN_POINT('Origin',(-0.115470053837925,0.,-1.38777878078145E-17));
#13852=CARTESIAN_POINT('',(-0.115470053837925,0.,-1.41410031829988E-17));
#13853=CARTESIAN_POINT('',(-0.0797862971081845,0.,-0.0618060796608387));
#13854=CARTESIAN_POINT('',(-0.115470053837925,-0.2,-1.38777878078145E-17));
#13855=CARTESIAN_POINT('',(-0.115470053837925,0.,-1.41410031829988E-17));
#13856=CARTESIAN_POINT('',(-0.0577350269189626,-0.2,-0.1));
#13857=CARTESIAN_POINT('Origin',(-0.0577350269189626,0.,0.1));
#13858=CARTESIAN_POINT('',(-0.0577350269189626,0.,0.1));
#13859=CARTESIAN_POINT('',(-0.0509187836487033,0.,0.111806079660839));
#13860=CARTESIAN_POINT('',(-0.0577350269189626,-0.2,0.1));
#13861=CARTESIAN_POINT('',(-0.0577350269189626,0.,0.1));
#13862=CARTESIAN_POINT('',(-0.115470053837925,-0.2,-1.41410031829988E-17));
#13863=CARTESIAN_POINT('Origin',(0.0577350269189626,0.,0.1));
#13864=CARTESIAN_POINT('',(0.0577350269189626,0.,0.1));
#13865=CARTESIAN_POINT('',(0.113867513459481,0.,0.1));
#13866=CARTESIAN_POINT('',(0.0577350269189626,-0.2,0.1));
#13867=CARTESIAN_POINT('',(0.0577350269189626,0.,0.1));
#13868=CARTESIAN_POINT('',(-0.0577350269189626,-0.2,0.1));
#13869=CARTESIAN_POINT('Origin',(0.115470053837925,0.,0.));
#13870=CARTESIAN_POINT('',(0.122286297108185,0.,-0.0118060796608386));
#13871=CARTESIAN_POINT('',(0.0577350269189626,-0.2,0.1));
#13872=CARTESIAN_POINT('Origin',(0.,-0.2,0.));
#13873=CARTESIAN_POINT('Origin',(0.17,0.,0.));
#13874=CARTESIAN_POINT('',(-0.17,-8.67361737988404E-18,-2.0818995585505E-17));
#13875=CARTESIAN_POINT('Origin',(0.,0.,0.));
#13876=CARTESIAN_POINT('Origin',(0.,-0.015,0.));
#13877=CARTESIAN_POINT('',(-0.1954,-0.0254,-2.39295984553393E-17));
#13878=CARTESIAN_POINT('Origin',(0.,-0.0254,0.));
#13879=CARTESIAN_POINT('',(-0.185,-0.015,-2.2655965784226E-17));
#13880=CARTESIAN_POINT('Origin',(0.,-0.2775,0.));
#13881=CARTESIAN_POINT('',(-0.1954,-0.5296,2.39295984553393E-17));
#13882=CARTESIAN_POINT('Origin',(0.,-0.5296,0.));
#13883=CARTESIAN_POINT('',(-0.1954,-0.2775,-2.39295984553393E-17));
#13884=CARTESIAN_POINT('Origin',(0.,-0.5625,0.));
#13885=CARTESIAN_POINT('',(-0.125,-0.6,-1.53080849893419E-17));
#13886=CARTESIAN_POINT('Origin',(0.,-0.6,0.));
#13887=CARTESIAN_POINT('',(-0.1625,-0.5625,-1.99005104861445E-17));
#13888=CARTESIAN_POINT('Origin',(0.,-0.6,0.));
#13889=CARTESIAN_POINT('',(0.,0.,0.));
#13890=CARTESIAN_POINT('Origin',(0.,-2.7,0.));
#13891=CARTESIAN_POINT('',(-0.289136645896019,-2.7,0.08));
#13892=CARTESIAN_POINT('',(-0.3,-2.78,-2.27065106771523E-17));
#13893=CARTESIAN_POINT('Ctrl Pts',(-0.289136645896019,-2.7,0.08));
#13894=CARTESIAN_POINT('Ctrl Pts',(-0.289136645896019,-2.71009877520201,
0.08));
#13895=CARTESIAN_POINT('Ctrl Pts',(-0.289720927595908,-2.72083518625944,
0.0779717130936404));
#13896=CARTESIAN_POINT('Ctrl Pts',(-0.291799203044223,-2.74052980652726,
0.0697927537456149));
#13897=CARTESIAN_POINT('Ctrl Pts',(-0.293259762986909,-2.74949254880105,
0.0636445361887959));
#13898=CARTESIAN_POINT('Ctrl Pts',(-0.295976783522942,-2.76364324458222,
0.0494938404076284));
#13899=CARTESIAN_POINT('Ctrl Pts',(-0.297414335384467,-2.76979246713824,
0.0405305642602551));
#13900=CARTESIAN_POINT('Ctrl Pts',(-0.299439403644655,-2.77797216257078,
0.0208340363410407));
#13901=CARTESIAN_POINT('Ctrl Pts',(-0.3,-2.78,0.0100969318362556));
#13902=CARTESIAN_POINT('Ctrl Pts',(-0.3,-2.78,5.20417042793042E-18));
#13903=CARTESIAN_POINT('',(0.289136645896019,-2.7,0.08));
#13904=CARTESIAN_POINT('',(0.,-2.7,0.08));
#13905=CARTESIAN_POINT('Ctrl Pts',(0.289136645896019,-2.7,0.08));
#13906=CARTESIAN_POINT('Ctrl Pts',(0.289136645896019,-2.68990122479799,
0.08));
#13907=CARTESIAN_POINT('Ctrl Pts',(0.289720927595908,-2.67916481374056,
0.0779717130936404));
#13908=CARTESIAN_POINT('Ctrl Pts',(0.291799203044223,-2.65947019347274,
0.0697927537456147));
#13909=CARTESIAN_POINT('Ctrl Pts',(0.293259762986909,-2.65050745119895,
0.0636445361887959));
#13910=CARTESIAN_POINT('Ctrl Pts',(0.295976783522942,-2.63635675541778,
0.0494938404076283));
#13911=CARTESIAN_POINT('Ctrl Pts',(0.297414335384467,-2.63020753286176,
0.0405305642602551));
#13912=CARTESIAN_POINT('Ctrl Pts',(0.299439403644655,-2.62202783742922,
0.0208340363410406));
#13913=CARTESIAN_POINT('Ctrl Pts',(0.3,-2.62,0.0100969318362555));
#13914=CARTESIAN_POINT('Ctrl Pts',(0.3,-2.62,-0.0100969318362556));
#13915=CARTESIAN_POINT('Ctrl Pts',(0.299439403644655,-2.62202783742922,
-0.0208340363410406));
#13916=CARTESIAN_POINT('Ctrl Pts',(0.297414335384467,-2.63020753286176,
-0.0405305642602551));
#13917=CARTESIAN_POINT('Ctrl Pts',(0.295976783522942,-2.63635675541778,
-0.0494938404076283));
#13918=CARTESIAN_POINT('Ctrl Pts',(0.293259762986909,-2.65050745119895,
-0.0636445361887959));
#13919=CARTESIAN_POINT('Ctrl Pts',(0.291799203044223,-2.65947019347274,
-0.0697927537456147));
#13920=CARTESIAN_POINT('Ctrl Pts',(0.289720927595908,-2.67916481374056,
-0.0779717130936403));
#13921=CARTESIAN_POINT('Ctrl Pts',(0.289136645896019,-2.68990122479799,
-0.08));
#13922=CARTESIAN_POINT('Ctrl Pts',(0.289136645896019,-2.71009877520201,
-0.08));
#13923=CARTESIAN_POINT('Ctrl Pts',(0.289720927595908,-2.72083518625944,
-0.0779717130936404));
#13924=CARTESIAN_POINT('Ctrl Pts',(0.291799203044223,-2.74052980652726,
-0.0697927537456147));
#13925=CARTESIAN_POINT('Ctrl Pts',(0.293259762986909,-2.74949254880105,
-0.0636445361887959));
#13926=CARTESIAN_POINT('Ctrl Pts',(0.295976783522942,-2.76364324458222,
-0.0494938404076283));
#13927=CARTESIAN_POINT('Ctrl Pts',(0.297414335384467,-2.76979246713824,
-0.0405305642602551));
#13928=CARTESIAN_POINT('Ctrl Pts',(0.299439403644655,-2.77797216257078,
-0.0208340363410406));
#13929=CARTESIAN_POINT('Ctrl Pts',(0.3,-2.78,-0.0100969318362555));
#13930=CARTESIAN_POINT('Ctrl Pts',(0.3,-2.78,0.0100969318362556));
#13931=CARTESIAN_POINT('Ctrl Pts',(0.299439403644655,-2.77797216257078,
0.0208340363410407));
#13932=CARTESIAN_POINT('Ctrl Pts',(0.297414335384467,-2.76979246713824,
0.0405305642602551));
#13933=CARTESIAN_POINT('Ctrl Pts',(0.295976783522942,-2.76364324458222,
0.0494938404076284));
#13934=CARTESIAN_POINT('Ctrl Pts',(0.293259762986909,-2.74949254880105,
0.0636445361887959));
#13935=CARTESIAN_POINT('Ctrl Pts',(0.291799203044223,-2.74052980652726,
0.0697927537456149));
#13936=CARTESIAN_POINT('Ctrl Pts',(0.289720927595908,-2.72083518625944,
0.0779717130936404));
#13937=CARTESIAN_POINT('Ctrl Pts',(0.289136645896019,-2.71009877520201,
0.08));
#13938=CARTESIAN_POINT('Ctrl Pts',(0.289136645896019,-2.7,0.08));
#13939=CARTESIAN_POINT('',(-0.3,-2.62,-3.65842984849668E-17));
#13940=CARTESIAN_POINT('Ctrl Pts',(-0.3,-2.62,-3.81639164714898E-17));
#13941=CARTESIAN_POINT('Ctrl Pts',(-0.3,-2.62,0.0100969318362555));
#13942=CARTESIAN_POINT('Ctrl Pts',(-0.299439403644655,-2.62202783742922,
0.0208340363410406));
#13943=CARTESIAN_POINT('Ctrl Pts',(-0.297414335384467,-2.63020753286176,
0.040530564260255));
#13944=CARTESIAN_POINT('Ctrl Pts',(-0.295976783522942,-2.63635675541778,
0.0494938404076283));
#13945=CARTESIAN_POINT('Ctrl Pts',(-0.293259762986909,-2.65050745119895,
0.0636445361887959));
#13946=CARTESIAN_POINT('Ctrl Pts',(-0.291799203044223,-2.65947019347274,
0.0697927537456147));
#13947=CARTESIAN_POINT('Ctrl Pts',(-0.289720927595908,-2.67916481374056,
0.0779717130936404));
#13948=CARTESIAN_POINT('Ctrl Pts',(-0.289136645896019,-2.68990122479799,
0.08));
#13949=CARTESIAN_POINT('Ctrl Pts',(-0.289136645896019,-2.7,0.08));
#13950=CARTESIAN_POINT('Ctrl Pts',(-0.3,-2.78,-6.93889390390723E-18));
#13951=CARTESIAN_POINT('Ctrl Pts',(-0.3,-2.78,-0.0100969318362556));
#13952=CARTESIAN_POINT('Ctrl Pts',(-0.299439403644655,-2.77797216257078,
-0.0208340363410406));
#13953=CARTESIAN_POINT('Ctrl Pts',(-0.297414335384467,-2.76979246713824,
-0.0405305642602551));
#13954=CARTESIAN_POINT('Ctrl Pts',(-0.295976783522942,-2.76364324458222,
-0.0494938404076283));
#13955=CARTESIAN_POINT('Ctrl Pts',(-0.293259762986909,-2.74949254880105,
-0.0636445361887959));
#13956=CARTESIAN_POINT('Ctrl Pts',(-0.291799203044223,-2.74052980652726,
-0.0697927537456147));
#13957=CARTESIAN_POINT('Ctrl Pts',(-0.289720927595908,-2.72083518625944,
-0.0779717130936403));
#13958=CARTESIAN_POINT('Ctrl Pts',(-0.289136645896019,-2.71009877520201,
-0.08));
#13959=CARTESIAN_POINT('Ctrl Pts',(-0.289136645896019,-2.68990122479799,
-0.08));
#13960=CARTESIAN_POINT('Ctrl Pts',(-0.289720927595908,-2.67916481374056,
-0.0779717130936403));
#13961=CARTESIAN_POINT('Ctrl Pts',(-0.291799203044223,-2.65947019347274,
-0.0697927537456147));
#13962=CARTESIAN_POINT('Ctrl Pts',(-0.293259762986909,-2.65050745119895,
-0.0636445361887959));
#13963=CARTESIAN_POINT('Ctrl Pts',(-0.295976783522942,-2.63635675541778,
-0.0494938404076283));
#13964=CARTESIAN_POINT('Ctrl Pts',(-0.297414335384467,-2.63020753286176,
-0.0405305642602551));
#13965=CARTESIAN_POINT('Ctrl Pts',(-0.299439403644655,-2.62202783742922,
-0.0208340363410406));
#13966=CARTESIAN_POINT('Ctrl Pts',(-0.3,-2.62,-0.0100969318362556));
#13967=CARTESIAN_POINT('Ctrl Pts',(-0.3,-2.62,-1.56125112837913E-17));
#13968=CARTESIAN_POINT('Origin',(0.45,0.2,0.));
#13969=CARTESIAN_POINT('',(-0.45,0.2,-5.51091059616309E-17));
#13970=CARTESIAN_POINT('Origin',(0.,0.2,0.));
#13971=CARTESIAN_POINT('Origin',(0.,0.175,0.));
#13972=CARTESIAN_POINT('',(-0.5,0.15,-6.12323399573676E-17));
#13973=CARTESIAN_POINT('Origin',(0.,0.15,0.));
#13974=CARTESIAN_POINT('',(-0.475,0.175,-5.81707229594993E-17));
#13975=CARTESIAN_POINT('Origin',(0.,0.0750000000000002,0.));
#13976=CARTESIAN_POINT('',(-0.5,0.,-6.12323399573677E-17));
#13977=CARTESIAN_POINT('Origin',(0.,0.,0.));
#13978=CARTESIAN_POINT('',(-0.5,0.0750000000000002,-6.12323399573677E-17));
#13979=CARTESIAN_POINT('Origin',(0.3,0.,0.));
#13980=CARTESIAN_POINT('',(-0.3,0.,-3.67394039744206E-17));
#13981=CARTESIAN_POINT('Origin',(0.,0.,0.));
#13982=CARTESIAN_POINT('Origin',(0.,-1.455,0.));
#13983=CARTESIAN_POINT('',(-0.3,-2.91,-3.67394039744206E-17));
#13984=CARTESIAN_POINT('Origin',(0.,-2.91,0.));
#13985=CARTESIAN_POINT('',(-0.3,-1.455,-3.67394039744206E-17));
#13986=CARTESIAN_POINT('',(-0.3,-1.455,-3.67394039744206E-17));
#13987=CARTESIAN_POINT('Origin',(0.,-2.955,0.));
#13988=CARTESIAN_POINT('',(-0.21,-3.,-2.57175827820944E-17));
#13989=CARTESIAN_POINT('Origin',(0.,-3.,0.));
#13990=CARTESIAN_POINT('',(-0.255,-2.955,-3.12284933782575E-17));
#13991=CARTESIAN_POINT('Origin',(0.,-3.,0.));
#13992=CARTESIAN_POINT('',(0.,0.,0.));
#13993=CARTESIAN_POINT('Origin',(0.,0.,0.));
#13994=CARTESIAN_POINT('',(-0.32,0.16,3.91886975727153E-17));
#13995=CARTESIAN_POINT('Origin',(0.,0.16,0.));
#13996=CARTESIAN_POINT('',(-0.32,0.,3.91886975727153E-17));
#13997=CARTESIAN_POINT('',(-0.32,0.,3.91886975727153E-17));
#13998=CARTESIAN_POINT('Origin',(0.,0.,0.));
#13999=CARTESIAN_POINT('Origin',(0.,0.,0.));
#14000=CARTESIAN_POINT('',(-0.6,0.16,7.34788079488412E-17));
#14001=CARTESIAN_POINT('Origin',(0.,0.16,0.));
#14002=CARTESIAN_POINT('',(-0.6,0.,7.34788079488412E-17));
#14003=CARTESIAN_POINT('',(-0.6,0.,7.34788079488412E-17));
#14004=CARTESIAN_POINT('Origin',(0.,0.,0.));
#14005=CARTESIAN_POINT('Origin',(0.,0.16,0.));
#14006=CARTESIAN_POINT('Origin',(0.,0.,0.));
#14007=CARTESIAN_POINT('',(0.,0.,0.));
#14008=CARTESIAN_POINT('Origin',(0.,0.12,0.));
#14009=CARTESIAN_POINT('',(-9.79717439317883E-18,0.12,-0.04));
#14010=CARTESIAN_POINT('Origin',(0.,0.12,-0.12));
#14011=CARTESIAN_POINT('Origin',(9.79717439317883E-18,0.12,0.));
#14012=CARTESIAN_POINT('',(0.08,-4.89858719658941E-18,7.34788079488412E-18));
#14013=CARTESIAN_POINT('',(-0.08,-4.89858719658941E-18,7.34788079488412E-18));
#14014=CARTESIAN_POINT('Ctrl Pts',(0.08,-4.89858719658941E-18,7.34788079488412E-18));
#14015=CARTESIAN_POINT('Ctrl Pts',(0.08,-0.00012864962353541,0.000128649623535413));
#14016=CARTESIAN_POINT('Ctrl Pts',(0.0799996896739287,-0.00025719571182076,
0.000257402596003253));
#14017=CARTESIAN_POINT('Ctrl Pts',(0.0799669711262291,-0.00701193164572964,
0.00703384588894362));
#14018=CARTESIAN_POINT('Ctrl Pts',(0.0791054994909294,-0.0133457972655825,
0.0139383126556792));
#14019=CARTESIAN_POINT('Ctrl Pts',(0.0749700088488058,-0.0265076530862524,
0.0292212026164895));
#14020=CARTESIAN_POINT('Ctrl Pts',(0.0712702072865517,-0.0331317062461458,
0.0375603420117568));
#14021=CARTESIAN_POINT('Ctrl Pts',(0.0612858949407667,-0.0440683985740427,
0.0520545604187517));
#14022=CARTESIAN_POINT('Ctrl Pts',(0.0555090276731744,-0.0485199197794574,
0.0582717815295611));
#14023=CARTESIAN_POINT('Ctrl Pts',(0.0412398082144208,-0.0561090538733877,
0.0691638397919718));
#14024=CARTESIAN_POINT('Ctrl Pts',(0.0327878980890048,-0.059089642483296,
0.0736229049587921));
#14025=CARTESIAN_POINT('Ctrl Pts',(0.0159233027310102,-0.0625179833270725,
0.0787936360751706));
#14026=CARTESIAN_POINT('Ctrl Pts',(0.00801661414593076,-0.0633030277982336,
0.08));
#14027=CARTESIAN_POINT('Ctrl Pts',(-0.00801661414593074,-0.0633030277982336,
0.08));
#14028=CARTESIAN_POINT('Ctrl Pts',(-0.0159233027310102,-0.0625179833270726,
0.0787936360751706));
#14029=CARTESIAN_POINT('Ctrl Pts',(-0.0327878980890049,-0.059089642483296,
0.0736229049587921));
#14030=CARTESIAN_POINT('Ctrl Pts',(-0.0412398082144209,-0.0561090538733877,
0.0691638397919717));
#14031=CARTESIAN_POINT('Ctrl Pts',(-0.0555090276731744,-0.0485199197794574,
0.0582717815295611));
#14032=CARTESIAN_POINT('Ctrl Pts',(-0.0612858949407667,-0.0440683985740427,
0.0520545604187517));
#14033=CARTESIAN_POINT('Ctrl Pts',(-0.0712702072865517,-0.0331317062461458,
0.0375603420117568));
#14034=CARTESIAN_POINT('Ctrl Pts',(-0.0749700088488058,-0.0265076530862524,
0.0292212026164895));
#14035=CARTESIAN_POINT('Ctrl Pts',(-0.0791054994909264,-0.0133457972655921,
0.0139383126556903));
#14036=CARTESIAN_POINT('Ctrl Pts',(-0.0799669711262287,-0.00701193164579759,
0.0070338458890125));
#14037=CARTESIAN_POINT('Ctrl Pts',(-0.0799996896739287,-0.000257195711817665,
0.000257402596000083));
#14038=CARTESIAN_POINT('Ctrl Pts',(-0.08,-0.000128649623538514,0.000128649623538516));
#14039=CARTESIAN_POINT('Ctrl Pts',(-0.08,-4.89858719658941E-18,7.34788079488412E-18));
#14040=CARTESIAN_POINT('Ctrl Pts',(-0.08,-4.89858719658941E-18,7.34788079488412E-18));
#14041=CARTESIAN_POINT('Ctrl Pts',(-0.08,-0.000128649623536042,-0.00012864962353603));
#14042=CARTESIAN_POINT('Ctrl Pts',(-0.0799996896739287,-0.000257195711820127,
-0.000257402596002604));
#14043=CARTESIAN_POINT('Ctrl Pts',(-0.0799669711262289,-0.0070119316457589,
-0.00703384588897312));
#14044=CARTESIAN_POINT('Ctrl Pts',(-0.0791054994909281,-0.0133457972655867,
-0.0139383126556841));
#14045=CARTESIAN_POINT('Ctrl Pts',(-0.0749700088488058,-0.0265076530862525,
-0.0292212026164896));
#14046=CARTESIAN_POINT('Ctrl Pts',(-0.0712702072865516,-0.0331317062461459,
-0.0375603420117568));
#14047=CARTESIAN_POINT('Ctrl Pts',(-0.0612858949407667,-0.0440683985740427,
-0.0520545604187517));
#14048=CARTESIAN_POINT('Ctrl Pts',(-0.0555090276731744,-0.0485199197794574,
-0.0582717815295611));
#14049=CARTESIAN_POINT('Ctrl Pts',(-0.0412398082144209,-0.0561090538733877,
-0.0691638397919717));
#14050=CARTESIAN_POINT('Ctrl Pts',(-0.0327878980890049,-0.059089642483296,
-0.0736229049587921));
#14051=CARTESIAN_POINT('Ctrl Pts',(-0.0159233027310101,-0.0625179833270725,
-0.0787936360751706));
#14052=CARTESIAN_POINT('Ctrl Pts',(-0.00801661414593069,-0.0633030277982336,
-0.08));
#14053=CARTESIAN_POINT('Ctrl Pts',(0.0080166141459307,-0.0633030277982336,
-0.08));
#14054=CARTESIAN_POINT('Ctrl Pts',(0.0159233027310101,-0.0625179833270725,
-0.0787936360751706));
#14055=CARTESIAN_POINT('Ctrl Pts',(0.0327878980890049,-0.0590896424832959,
-0.0736229049587921));
#14056=CARTESIAN_POINT('Ctrl Pts',(0.0412398082144209,-0.0561090538733877,
-0.0691638397919717));
#14057=CARTESIAN_POINT('Ctrl Pts',(0.0555090276731744,-0.0485199197794574,
-0.0582717815295611));
#14058=CARTESIAN_POINT('Ctrl Pts',(0.0612858949407666,-0.0440683985740428,
-0.0520545604187518));
#14059=CARTESIAN_POINT('Ctrl Pts',(0.0712702072865517,-0.0331317062461458,
-0.0375603420117568));
#14060=CARTESIAN_POINT('Ctrl Pts',(0.0749700088488058,-0.0265076530862524,
-0.0292212026164895));
#14061=CARTESIAN_POINT('Ctrl Pts',(0.079105499490928,-0.013345797265587,
-0.0139383126556845));
#14062=CARTESIAN_POINT('Ctrl Pts',(0.0799669711262289,-0.00701193164576148,
-0.00703384588897579));
#14063=CARTESIAN_POINT('Ctrl Pts',(0.0799996896739287,-0.000257195711819584,
-0.000257402596002039));
#14064=CARTESIAN_POINT('Ctrl Pts',(0.08,-0.000128649623536605,-0.000128649623536593));
#14065=CARTESIAN_POINT('Ctrl Pts',(0.08,-4.89858719658941E-18,7.34788079488412E-18));
#14066=CARTESIAN_POINT('Origin',(0.04,-1.36,0.));
#14067=CARTESIAN_POINT('',(0.,-1.36,-0.08));
#14068=CARTESIAN_POINT('',(0.,-1.36,0.08));
#14069=CARTESIAN_POINT('Origin',(0.,-1.36,0.));
#14070=CARTESIAN_POINT('',(0.,-1.36,-0.04));
#14071=CARTESIAN_POINT('Origin',(0.,0.,-0.08));
#14072=CARTESIAN_POINT('',(0.,-1.6,0.08));
#14073=CARTESIAN_POINT('',(0.,0.,0.08));
#14074=CARTESIAN_POINT('',(0.,-1.6,-0.08));
#14075=CARTESIAN_POINT('',(0.,-1.6,-0.09));
#14076=CARTESIAN_POINT('',(0.,0.,-0.08));
#14077=CARTESIAN_POINT('Origin',(0.,0.,0.));
#14078=CARTESIAN_POINT('',(-0.08,-1.6,-9.79717439317883E-18));
#14079=CARTESIAN_POINT('Origin',(0.,-1.6,0.));
#14080=CARTESIAN_POINT('',(-0.08,0.,-9.79717439317883E-18));
#14081=CARTESIAN_POINT('Origin',(0.,-1.6,0.));
#14082=CARTESIAN_POINT('Origin',(-0.04,-1.6,0.));
#14083=CARTESIAN_POINT('',(0.,0.,0.));
#14084=CARTESIAN_POINT('Origin',(-5.,-9.4,4.5));
#14085=CARTESIAN_POINT('',(-5.3,-7.4,4.5));
#14086=CARTESIAN_POINT('Origin',(-5.,-7.4,4.5));
#14087=CARTESIAN_POINT('',(-5.3,-9.4,4.5));
#14088=CARTESIAN_POINT('',(-5.3,-9.4,4.5));
#14089=CARTESIAN_POINT('Origin',(-5.,-9.4,4.5));
#14090=CARTESIAN_POINT('Origin',(-5.,-9.4,4.5));
#14091=CARTESIAN_POINT('Origin',(-5.,-7.4,4.5));
#14092=CARTESIAN_POINT('',(-5.6,9.8,4.5));
#14093=CARTESIAN_POINT('Origin',(-5.,9.8,4.5));
#14094=CARTESIAN_POINT('',(-5.6,-7.4,4.5));
#14095=CARTESIAN_POINT('',(-5.6,-7.4,4.5));
#14096=CARTESIAN_POINT('Origin',(-5.,-7.4,4.5));
#14097=CARTESIAN_POINT('Origin',(-5.,9.8,4.5));
#14098=CARTESIAN_POINT('Origin',(-5.,-7.4,4.5));
#14099=CARTESIAN_POINT('',(0.,0.,0.));
#14100=CARTESIAN_POINT('Origin',(5.,-9.4,4.5));
#14101=CARTESIAN_POINT('',(4.7,-7.4,4.5));
#14102=CARTESIAN_POINT('Origin',(5.,-7.4,4.5));
#14103=CARTESIAN_POINT('',(4.7,-9.4,4.5));
#14104=CARTESIAN_POINT('',(4.7,-9.4,4.5));
#14105=CARTESIAN_POINT('Origin',(5.,-9.4,4.5));
#14106=CARTESIAN_POINT('Origin',(5.,-9.4,4.5));
#14107=CARTESIAN_POINT('Origin',(5.,-7.4,4.5));
#14108=CARTESIAN_POINT('',(4.4,9.8,4.5));
#14109=CARTESIAN_POINT('Origin',(5.,9.8,4.5));
#14110=CARTESIAN_POINT('',(4.4,-7.4,4.5));
#14111=CARTESIAN_POINT('',(4.4,-7.4,4.5));
#14112=CARTESIAN_POINT('Origin',(5.,-7.4,4.5));
#14113=CARTESIAN_POINT('Origin',(5.,9.8,4.5));
#14114=CARTESIAN_POINT('Origin',(5.,-7.4,4.5));
#14115=CARTESIAN_POINT('',(0.,0.,0.));
#14116=CARTESIAN_POINT('Origin',(-5.,-8.5,4.5));
#14117=CARTESIAN_POINT('',(-5.325,-8.4,4.5));
#14118=CARTESIAN_POINT('Origin',(-5.,-8.4,4.5));
#14119=CARTESIAN_POINT('',(-5.325,-7.4,4.5));
#14120=CARTESIAN_POINT('',(-5.325,-8.5,4.5));
#14121=CARTESIAN_POINT('Origin',(-5.,-7.4,4.5));
#14122=CARTESIAN_POINT('Origin',(5.,-8.5,4.5));
#14123=CARTESIAN_POINT('',(4.675,-8.4,4.5));
#14124=CARTESIAN_POINT('Origin',(5.,-8.4,4.5));
#14125=CARTESIAN_POINT('',(4.675,-7.4,4.5));
#14126=CARTESIAN_POINT('',(4.675,-8.5,4.5));
#14127=CARTESIAN_POINT('Origin',(5.,-7.4,4.5));
#14128=CARTESIAN_POINT('Origin',(-0.6,-6.1,4.5));
#14129=CARTESIAN_POINT('',(-0.48,-6.1,4.81));
#14130=CARTESIAN_POINT('Origin',(-0.48,-6.1,4.5));
#14131=CARTESIAN_POINT('',(0.48,-6.1,4.81));
#14132=CARTESIAN_POINT('',(-0.6,-6.1,4.81));
#14133=CARTESIAN_POINT('Origin',(0.48,-6.1,4.5));
#14134=CARTESIAN_POINT('Origin',(0.,-7.01,3.9));
#14135=CARTESIAN_POINT('',(-0.48,-7.4,3.9));
#14136=CARTESIAN_POINT('',(0.48,-7.4,3.9));
#14137=CARTESIAN_POINT('',(3.25,-7.4,3.9));
#14138=CARTESIAN_POINT('',(-0.48,-5.62,3.9));
#14139=CARTESIAN_POINT('',(-0.48,-5.62,3.9));
#14140=CARTESIAN_POINT('',(0.48,-5.62,3.9));
#14141=CARTESIAN_POINT('',(0.48,-5.62,3.9));
#14142=CARTESIAN_POINT('',(0.48,-8.4,3.9));
#14143=CARTESIAN_POINT('Origin',(-0.48,-5.62,3.9));
#14144=CARTESIAN_POINT('',(-0.48,-7.4,5.1));
#14145=CARTESIAN_POINT('',(-0.48,-7.4,3.45));
#14146=CARTESIAN_POINT('',(-0.48,-5.62,5.1));
#14147=CARTESIAN_POINT('',(-0.48,-5.62,5.1));
#14148=CARTESIAN_POINT('',(-0.48,-5.62,3.9));
#14149=CARTESIAN_POINT('Origin',(0.48,-5.62,3.9));
#14150=CARTESIAN_POINT('',(0.48,-5.62,5.1));
#14151=CARTESIAN_POINT('',(0.48,-5.62,5.1));
#14152=CARTESIAN_POINT('',(0.48,-5.62,3.9));
#14153=CARTESIAN_POINT('Origin',(0.48,-8.4,3.9));
#14154=CARTESIAN_POINT('',(0.48,-7.4,5.1));
#14155=CARTESIAN_POINT('',(0.48,-7.4,3.45));
#14156=CARTESIAN_POINT('',(0.48,-8.4,5.1));
#14157=CARTESIAN_POINT('Origin',(0.,-7.01,5.1));
#14158=CARTESIAN_POINT('',(3.25,-7.4,5.1));
#14159=CARTESIAN_POINT('Origin',(6.5,-7.4,3.));
#14160=CARTESIAN_POINT('',(6.5,-7.4,3.));
#14161=CARTESIAN_POINT('',(-6.5,-7.4,3.));
#14162=CARTESIAN_POINT('',(6.5,-7.4,3.));
#14163=CARTESIAN_POINT('',(-6.5,-7.4,6.));
#14164=CARTESIAN_POINT('',(-6.5,-7.4,3.));
#14165=CARTESIAN_POINT('',(6.5,-7.4,6.));
#14166=CARTESIAN_POINT('',(6.5,-7.4,6.));
#14167=CARTESIAN_POINT('',(6.5,-7.4,3.));
#14168=CARTESIAN_POINT('Origin',(6.5,-8.4,3.));
#14169=CARTESIAN_POINT('',(6.5,-8.4,3.));
#14170=CARTESIAN_POINT('',(6.5,-8.4,3.));
#14171=CARTESIAN_POINT('',(6.5,-8.4,6.));
#14172=CARTESIAN_POINT('',(6.5,-8.4,6.));
#14173=CARTESIAN_POINT('',(6.5,-8.4,3.));
#14174=CARTESIAN_POINT('Origin',(-6.5,-8.4,3.));
#14175=CARTESIAN_POINT('',(-6.5,-8.4,3.));
#14176=CARTESIAN_POINT('',(-6.5,-8.4,3.));
#14177=CARTESIAN_POINT('',(-6.5,-8.4,6.));
#14178=CARTESIAN_POINT('',(-6.5,-8.4,6.));
#14179=CARTESIAN_POINT('',(-6.5,-8.4,3.));
#14180=CARTESIAN_POINT('Origin',(-6.5,-7.4,3.));
#14181=CARTESIAN_POINT('',(-6.5,-7.4,3.));
#14182=CARTESIAN_POINT('',(-6.5,-7.4,6.));
#14183=CARTESIAN_POINT('Origin',(0.,-7.9,6.));
#14184=CARTESIAN_POINT('Origin',(0.,-7.9,3.));
#14185=CARTESIAN_POINT('',(0.,0.,0.));
#14186=CARTESIAN_POINT('Origin',(0.,0.,0.));
#14187=CARTESIAN_POINT('',(-0.32,0.16,3.91886975727153E-17));
#14188=CARTESIAN_POINT('Origin',(0.,0.16,0.));
#14189=CARTESIAN_POINT('',(-0.32,0.,3.91886975727153E-17));
#14190=CARTESIAN_POINT('',(-0.32,0.,3.91886975727153E-17));
#14191=CARTESIAN_POINT('Origin',(0.,0.,0.));
#14192=CARTESIAN_POINT('Origin',(0.,0.,0.));
#14193=CARTESIAN_POINT('',(-0.6,0.16,7.34788079488412E-17));
#14194=CARTESIAN_POINT('Origin',(0.,0.16,0.));
#14195=CARTESIAN_POINT('',(-0.6,0.,7.34788079488412E-17));
#14196=CARTESIAN_POINT('',(-0.6,0.,7.34788079488412E-17));
#14197=CARTESIAN_POINT('Origin',(0.,0.,0.));
#14198=CARTESIAN_POINT('Origin',(0.,0.16,0.));
#14199=CARTESIAN_POINT('Origin',(0.,0.,0.));
#14200=CARTESIAN_POINT('',(0.,0.,0.));
#14201=CARTESIAN_POINT('Origin',(0.,0.0584134911936118,0.));
#14202=CARTESIAN_POINT('',(-0.288675134594813,0.0590919554682611,0.5));
#14203=CARTESIAN_POINT('',(0.288675134594813,0.0590919554682611,0.5));
#14204=CARTESIAN_POINT('Ctrl Pts',(-0.288675134594813,0.0590919554682611,
0.5));
#14205=CARTESIAN_POINT('Ctrl Pts',(2.1664336991023E-12,-0.0242413778636964,
0.5));
#14206=CARTESIAN_POINT('Ctrl Pts',(0.288675134594813,0.0590919554682611,
0.5));
#14207=CARTESIAN_POINT('',(-0.577350269189626,0.0590919554682611,-7.07050159149938E-17));
#14208=CARTESIAN_POINT('Ctrl Pts',(-0.577350269189626,0.0590919554682611,
-7.07050159149938E-17));
#14209=CARTESIAN_POINT('Ctrl Pts',(-0.433012701891136,-0.0242413778636963,
0.250000000001876));
#14210=CARTESIAN_POINT('Ctrl Pts',(-0.288675134594813,0.0590919554682611,
0.5));
#14211=CARTESIAN_POINT('',(-0.475,-4.16333634234434E-17,-5.81707229594993E-17));
#14212=CARTESIAN_POINT('',(-0.576175134594813,0.0584134911936118,-7.05611034329833E-17));
#14213=CARTESIAN_POINT('Origin',(0.,0.,0.));
#14214=CARTESIAN_POINT('',(-0.288675134594813,0.0590919554682611,-0.5));
#14215=CARTESIAN_POINT('Ctrl Pts',(-0.288675134594813,0.0590919554682611,
-0.5));
#14216=CARTESIAN_POINT('Ctrl Pts',(-0.433012701893303,-0.0242413778636963,
-0.249999999998124));
#14217=CARTESIAN_POINT('Ctrl Pts',(-0.577350269189626,0.0590919554682611,
-7.07050159149938E-17));
#14218=CARTESIAN_POINT('',(0.288675134594813,0.0590919554682611,-0.5));
#14219=CARTESIAN_POINT('Ctrl Pts',(0.288675134594813,0.0590919554682611,
-0.5));
#14220=CARTESIAN_POINT('Ctrl Pts',(-2.16648921025353E-12,-0.0242413778636962,
-0.5));
#14221=CARTESIAN_POINT('Ctrl Pts',(-0.288675134594813,0.0590919554682611,
-0.5));
#14222=CARTESIAN_POINT('',(0.577350269189626,0.0590919554682611,0.));
#14223=CARTESIAN_POINT('Ctrl Pts',(0.577350269189626,0.0590919554682611,
0.));
#14224=CARTESIAN_POINT('Ctrl Pts',(0.433012701891136,-0.0242413778636963,
-0.250000000001876));
#14225=CARTESIAN_POINT('Ctrl Pts',(0.288675134594813,0.0590919554682611,
-0.5));
#14226=CARTESIAN_POINT('Ctrl Pts',(0.288675134594813,0.0590919554682611,
0.5));
#14227=CARTESIAN_POINT('Ctrl Pts',(0.433012701893303,-0.0242413778636962,
0.249999999998124));
#14228=CARTESIAN_POINT('Ctrl Pts',(0.577350269189626,0.0590919554682611,
0.));
#14229=CARTESIAN_POINT('Origin',(0.,0.461586508806388,0.));
#14230=CARTESIAN_POINT('',(-0.475,0.52,-5.81707229594993E-17));
#14231=CARTESIAN_POINT('Origin',(0.,0.52,0.));
#14232=CARTESIAN_POINT('',(-0.577350269189626,0.460908044531739,-7.07050159149938E-17));
#14233=CARTESIAN_POINT('',(-0.576175134594813,0.461586508806388,-7.05611034329833E-17));
#14234=CARTESIAN_POINT('',(-0.288675134594813,0.460908044531739,0.5));
#14235=CARTESIAN_POINT('Ctrl Pts',(-0.288675134594813,0.460908044531739,
0.5));
#14236=CARTESIAN_POINT('Ctrl Pts',(-0.433012701893303,0.544241377863696,
0.249999999998124));
#14237=CARTESIAN_POINT('Ctrl Pts',(-0.577350269189626,0.460908044531739,
-7.07050159149938E-17));
#14238=CARTESIAN_POINT('',(0.288675134594813,0.460908044531739,0.5));
#14239=CARTESIAN_POINT('Ctrl Pts',(0.288675134594813,0.460908044531739,
0.5));
#14240=CARTESIAN_POINT('Ctrl Pts',(-2.16676676600969E-12,0.544241377863697,
0.5));
#14241=CARTESIAN_POINT('Ctrl Pts',(-0.288675134594813,0.460908044531739,
0.5));
#14242=CARTESIAN_POINT('',(0.577350269189626,0.460908044531739,0.));
#14243=CARTESIAN_POINT('Ctrl Pts',(0.577350269189626,0.460908044531739,
0.));
#14244=CARTESIAN_POINT('Ctrl Pts',(0.433012701891136,0.544241377863696,
0.250000000001876));
#14245=CARTESIAN_POINT('Ctrl Pts',(0.288675134594813,0.460908044531739,
0.5));
#14246=CARTESIAN_POINT('',(0.288675134594813,0.460908044531739,-0.5));
#14247=CARTESIAN_POINT('Ctrl Pts',(0.288675134594813,0.460908044531739,
-0.5));
#14248=CARTESIAN_POINT('Ctrl Pts',(0.433012701893302,0.544241377863696,
-0.249999999998124));
#14249=CARTESIAN_POINT('Ctrl Pts',(0.577350269189626,0.460908044531739,
0.));
#14250=CARTESIAN_POINT('',(-0.288675134594813,0.460908044531739,-0.5));
#14251=CARTESIAN_POINT('Ctrl Pts',(-0.288675134594813,0.460908044531739,
-0.5));
#14252=CARTESIAN_POINT('Ctrl Pts',(2.16660023255599E-12,0.544241377863697,
-0.5));
#14253=CARTESIAN_POINT('Ctrl Pts',(0.288675134594813,0.460908044531739,
-0.5));
#14254=CARTESIAN_POINT('Ctrl Pts',(-0.577350269189626,0.460908044531739,
-7.07050159149938E-17));
#14255=CARTESIAN_POINT('Ctrl Pts',(-0.433012701891136,0.544241377863696,
-0.250000000001876));
#14256=CARTESIAN_POINT('Ctrl Pts',(-0.288675134594813,0.460908044531739,
-0.5));
#14257=CARTESIAN_POINT('Origin',(0.288675134594813,0.,-0.5));
#14258=CARTESIAN_POINT('',(-0.288675134594813,0.,-0.5));
#14259=CARTESIAN_POINT('',(0.288675134594813,0.,-0.5));
#14260=CARTESIAN_POINT('Origin',(-0.288675134594813,0.,-0.5));
#14261=CARTESIAN_POINT('',(-0.577350269189626,0.,-7.07050159149938E-17));
#14262=CARTESIAN_POINT('Origin',(-0.577350269189626,0.,-7.07050159149938E-17));
#14263=CARTESIAN_POINT('',(-0.288675134594813,0.,0.5));
#14264=CARTESIAN_POINT('Origin',(0.,0.,0.));
#14265=CARTESIAN_POINT('',(-0.25175,0.52,3.08304831685346E-17));
#14266=CARTESIAN_POINT('Origin',(0.,0.52,0.));
#14267=CARTESIAN_POINT('',(-0.25175,0.,3.08304831685346E-17));
#14268=CARTESIAN_POINT('',(-0.25175,0.,3.08304831685346E-17));
#14269=CARTESIAN_POINT('Origin',(0.,0.,0.));
#14270=CARTESIAN_POINT('Origin',(-0.288675134594813,0.,0.5));
#14271=CARTESIAN_POINT('',(0.288675134594813,0.,0.5));
#14272=CARTESIAN_POINT('Origin',(0.577350269189626,0.,0.));
#14273=CARTESIAN_POINT('',(0.577350269189626,0.,0.));
#14274=CARTESIAN_POINT('Origin',(0.288675134594813,0.,0.5));
#14275=CARTESIAN_POINT('Origin',(0.,0.52,0.));
#14276=CARTESIAN_POINT('Origin',(0.,0.,0.));
#14277=CARTESIAN_POINT('',(0.,0.,0.));
#14278=CARTESIAN_POINT('',(0.,0.,0.));
#14279=CARTESIAN_POINT('',(0.,0.,0.));
#14280=CARTESIAN_POINT('',(0.,3.2,4.5));
#14281=CARTESIAN_POINT('',(0.,0.,0.));
#14282=CARTESIAN_POINT('',(0.,-5.3,5.5));
#14283=CARTESIAN_POINT('',(-1.16,-6.1,4.5));
#14284=CARTESIAN_POINT('',(-1.16,-6.1,4.5));
#14285=CARTESIAN_POINT('',(1.,-6.1,4.5));
#14286=CARTESIAN_POINT('',(1.16,-6.1,4.5));
#14287=CARTESIAN_POINT('',(1.54,-5.7,4.5));
#14288=CARTESIAN_POINT('',(0.,0.,0.));
#14289=CARTESIAN_POINT('',(0.,0.,0.));
#14290=CARTESIAN_POINT('',(0.,0.,0.));
#14291=CARTESIAN_POINT('',(-5.,-8.56,4.5));
#14292=CARTESIAN_POINT('',(-5.,-9.08,4.5));
#14293=CARTESIAN_POINT('',(5.,-8.56,4.5));
#14294=CARTESIAN_POINT('',(5.,-9.08,4.5));
#14295=CARTESIAN_POINT('',(0.,0.,0.));
#14296=CARTESIAN_POINT('',(0.,0.,0.));
#14297=UNCERTAINTY_MEASURE_WITH_UNIT(LENGTH_MEASURE(0.001),#14393,
'DISTANCE_ACCURACY_VALUE',
'Maximum model space distance between geometric entities at asserted c
onnectivities');
#14298=UNCERTAINTY_MEASURE_WITH_UNIT(LENGTH_MEASURE(0.001),#14393,
'DISTANCE_ACCURACY_VALUE',
'Maximum model space distance between geometric entities at asserted c
onnectivities');
#14299=UNCERTAINTY_MEASURE_WITH_UNIT(LENGTH_MEASURE(0.001),#14393,
'DISTANCE_ACCURACY_VALUE',
'Maximum model space distance between geometric entities at asserted c
onnectivities');
#14300=UNCERTAINTY_MEASURE_WITH_UNIT(LENGTH_MEASURE(0.001),#14393,
'DISTANCE_ACCURACY_VALUE',
'Maximum model space distance between geometric entities at asserted c
onnectivities');
#14301=UNCERTAINTY_MEASURE_WITH_UNIT(LENGTH_MEASURE(0.001),#14393,
'DISTANCE_ACCURACY_VALUE',
'Maximum model space distance between geometric entities at asserted c
onnectivities');
#14302=UNCERTAINTY_MEASURE_WITH_UNIT(LENGTH_MEASURE(0.001),#14393,
'DISTANCE_ACCURACY_VALUE',
'Maximum model space distance between geometric entities at asserted c
onnectivities');
#14303=UNCERTAINTY_MEASURE_WITH_UNIT(LENGTH_MEASURE(0.001),#14393,
'DISTANCE_ACCURACY_VALUE',
'Maximum model space distance between geometric entities at asserted c
onnectivities');
#14304=UNCERTAINTY_MEASURE_WITH_UNIT(LENGTH_MEASURE(0.001),#14393,
'DISTANCE_ACCURACY_VALUE',
'Maximum model space distance between geometric entities at asserted c
onnectivities');
#14305=UNCERTAINTY_MEASURE_WITH_UNIT(LENGTH_MEASURE(0.001),#14393,
'DISTANCE_ACCURACY_VALUE',
'Maximum model space distance between geometric entities at asserted c
onnectivities');
#14306=UNCERTAINTY_MEASURE_WITH_UNIT(LENGTH_MEASURE(0.001),#14393,
'DISTANCE_ACCURACY_VALUE',
'Maximum model space distance between geometric entities at asserted c
onnectivities');
#14307=UNCERTAINTY_MEASURE_WITH_UNIT(LENGTH_MEASURE(0.001),#14393,
'DISTANCE_ACCURACY_VALUE',
'Maximum model space distance between geometric entities at asserted c
onnectivities');
#14308=UNCERTAINTY_MEASURE_WITH_UNIT(LENGTH_MEASURE(0.001),#14393,
'DISTANCE_ACCURACY_VALUE',
'Maximum model space distance between geometric entities at asserted c
onnectivities');
#14309=UNCERTAINTY_MEASURE_WITH_UNIT(LENGTH_MEASURE(0.001),#14393,
'DISTANCE_ACCURACY_VALUE',
'Maximum model space distance between geometric entities at asserted c
onnectivities');
#14310=UNCERTAINTY_MEASURE_WITH_UNIT(LENGTH_MEASURE(0.001),#14393,
'DISTANCE_ACCURACY_VALUE',
'Maximum model space distance between geometric entities at asserted c
onnectivities');
#14311=UNCERTAINTY_MEASURE_WITH_UNIT(LENGTH_MEASURE(0.001),#14393,
'DISTANCE_ACCURACY_VALUE',
'Maximum model space distance between geometric entities at asserted c
onnectivities');
#14312=UNCERTAINTY_MEASURE_WITH_UNIT(LENGTH_MEASURE(0.001),#14393,
'DISTANCE_ACCURACY_VALUE',
'Maximum model space distance between geometric entities at asserted c
onnectivities');
#14313=UNCERTAINTY_MEASURE_WITH_UNIT(LENGTH_MEASURE(0.001),#14393,
'DISTANCE_ACCURACY_VALUE',
'Maximum model space distance between geometric entities at asserted c
onnectivities');
#14314=UNCERTAINTY_MEASURE_WITH_UNIT(LENGTH_MEASURE(0.001),#14393,
'DISTANCE_ACCURACY_VALUE',
'Maximum model space distance between geometric entities at asserted c
onnectivities');
#14315=UNCERTAINTY_MEASURE_WITH_UNIT(LENGTH_MEASURE(0.001),#14393,
'DISTANCE_ACCURACY_VALUE',
'Maximum model space distance between geometric entities at asserted c
onnectivities');
#14316=UNCERTAINTY_MEASURE_WITH_UNIT(LENGTH_MEASURE(0.001),#14393,
'DISTANCE_ACCURACY_VALUE',
'Maximum model space distance between geometric entities at asserted c
onnectivities');
#14317=UNCERTAINTY_MEASURE_WITH_UNIT(LENGTH_MEASURE(0.001),#14393,
'DISTANCE_ACCURACY_VALUE',
'Maximum model space distance between geometric entities at asserted c
onnectivities');
#14318=UNCERTAINTY_MEASURE_WITH_UNIT(LENGTH_MEASURE(0.001),#14393,
'DISTANCE_ACCURACY_VALUE',
'Maximum model space distance between geometric entities at asserted c
onnectivities');
#14319=UNCERTAINTY_MEASURE_WITH_UNIT(LENGTH_MEASURE(0.001),#14393,
'DISTANCE_ACCURACY_VALUE',
'Maximum model space distance between geometric entities at asserted c
onnectivities');
#14320=UNCERTAINTY_MEASURE_WITH_UNIT(LENGTH_MEASURE(0.001),#14393,
'DISTANCE_ACCURACY_VALUE',
'Maximum model space distance between geometric entities at asserted c
onnectivities');
#14321=UNCERTAINTY_MEASURE_WITH_UNIT(LENGTH_MEASURE(0.001),#14393,
'DISTANCE_ACCURACY_VALUE',
'Maximum model space distance between geometric entities at asserted c
onnectivities');
#14322=UNCERTAINTY_MEASURE_WITH_UNIT(LENGTH_MEASURE(0.001),#14393,
'DISTANCE_ACCURACY_VALUE',
'Maximum model space distance between geometric entities at asserted c
onnectivities');
#14323=UNCERTAINTY_MEASURE_WITH_UNIT(LENGTH_MEASURE(0.001),#14393,
'DISTANCE_ACCURACY_VALUE',
'Maximum model space distance between geometric entities at asserted c
onnectivities');
#14324=UNCERTAINTY_MEASURE_WITH_UNIT(LENGTH_MEASURE(0.001),#14393,
'DISTANCE_ACCURACY_VALUE',
'Maximum model space distance between geometric entities at asserted c
onnectivities');
#14325=UNCERTAINTY_MEASURE_WITH_UNIT(LENGTH_MEASURE(0.001),#14393,
'DISTANCE_ACCURACY_VALUE',
'Maximum model space distance between geometric entities at asserted c
onnectivities');
#14326=UNCERTAINTY_MEASURE_WITH_UNIT(LENGTH_MEASURE(0.001),#14393,
'DISTANCE_ACCURACY_VALUE',
'Maximum model space distance between geometric entities at asserted c
onnectivities');
#14327=UNCERTAINTY_MEASURE_WITH_UNIT(LENGTH_MEASURE(0.001),#14393,
'DISTANCE_ACCURACY_VALUE',
'Maximum model space distance between geometric entities at asserted c
onnectivities');
#14328=UNCERTAINTY_MEASURE_WITH_UNIT(LENGTH_MEASURE(0.001),#14393,
'DISTANCE_ACCURACY_VALUE',
'Maximum model space distance between geometric entities at asserted c
onnectivities');
#14329=UNCERTAINTY_MEASURE_WITH_UNIT(LENGTH_MEASURE(0.001),#14393,
'DISTANCE_ACCURACY_VALUE',
'Maximum model space distance between geometric entities at asserted c
onnectivities');
#14330=UNCERTAINTY_MEASURE_WITH_UNIT(LENGTH_MEASURE(0.001),#14393,
'DISTANCE_ACCURACY_VALUE',
'Maximum model space distance between geometric entities at asserted c
onnectivities');
#14331=UNCERTAINTY_MEASURE_WITH_UNIT(LENGTH_MEASURE(0.001),#14393,
'DISTANCE_ACCURACY_VALUE',
'Maximum model space distance between geometric entities at asserted c
onnectivities');
#14332=UNCERTAINTY_MEASURE_WITH_UNIT(LENGTH_MEASURE(0.001),#14393,
'DISTANCE_ACCURACY_VALUE',
'Maximum model space distance between geometric entities at asserted c
onnectivities');
#14333=UNCERTAINTY_MEASURE_WITH_UNIT(LENGTH_MEASURE(0.001),#14393,
'DISTANCE_ACCURACY_VALUE',
'Maximum model space distance between geometric entities at asserted c
onnectivities');
#14334=UNCERTAINTY_MEASURE_WITH_UNIT(LENGTH_MEASURE(0.001),#14393,
'DISTANCE_ACCURACY_VALUE',
'Maximum model space distance between geometric entities at asserted c
onnectivities');
#14335=UNCERTAINTY_MEASURE_WITH_UNIT(LENGTH_MEASURE(0.001),#14393,
'DISTANCE_ACCURACY_VALUE',
'Maximum model space distance between geometric entities at asserted c
onnectivities');
#14336=UNCERTAINTY_MEASURE_WITH_UNIT(LENGTH_MEASURE(0.001),#14393,
'DISTANCE_ACCURACY_VALUE',
'Maximum model space distance between geometric entities at asserted c
onnectivities');
#14337=UNCERTAINTY_MEASURE_WITH_UNIT(LENGTH_MEASURE(0.001),#14393,
'DISTANCE_ACCURACY_VALUE',
'Maximum model space distance between geometric entities at asserted c
onnectivities');
#14338=UNCERTAINTY_MEASURE_WITH_UNIT(LENGTH_MEASURE(0.001),#14393,
'DISTANCE_ACCURACY_VALUE',
'Maximum model space distance between geometric entities at asserted c
onnectivities');
#14339=UNCERTAINTY_MEASURE_WITH_UNIT(LENGTH_MEASURE(0.001),#14393,
'DISTANCE_ACCURACY_VALUE',
'Maximum model space distance between geometric entities at asserted c
onnectivities');
#14340=UNCERTAINTY_MEASURE_WITH_UNIT(LENGTH_MEASURE(0.001),#14393,
'DISTANCE_ACCURACY_VALUE',
'Maximum model space distance between geometric entities at asserted c
onnectivities');
#14341=UNCERTAINTY_MEASURE_WITH_UNIT(LENGTH_MEASURE(0.001),#14393,
'DISTANCE_ACCURACY_VALUE',
'Maximum model space distance between geometric entities at asserted c
onnectivities');
#14342=UNCERTAINTY_MEASURE_WITH_UNIT(LENGTH_MEASURE(0.001),#14393,
'DISTANCE_ACCURACY_VALUE',
'Maximum model space distance between geometric entities at asserted c
onnectivities');
#14343=UNCERTAINTY_MEASURE_WITH_UNIT(LENGTH_MEASURE(0.001),#14393,
'DISTANCE_ACCURACY_VALUE',
'Maximum model space distance between geometric entities at asserted c
onnectivities');
#14344=UNCERTAINTY_MEASURE_WITH_UNIT(LENGTH_MEASURE(0.001),#14393,
'DISTANCE_ACCURACY_VALUE',
'Maximum model space distance between geometric entities at asserted c
onnectivities');
#14345=(
GEOMETRIC_REPRESENTATION_CONTEXT(3)
GLOBAL_UNCERTAINTY_ASSIGNED_CONTEXT((#14297))
GLOBAL_UNIT_ASSIGNED_CONTEXT((#14393,#14395,#14396))
REPRESENTATION_CONTEXT('','3D')
);
#14346=(
GEOMETRIC_REPRESENTATION_CONTEXT(3)
GLOBAL_UNCERTAINTY_ASSIGNED_CONTEXT((#14298))
GLOBAL_UNIT_ASSIGNED_CONTEXT((#14393,#14395,#14396))
REPRESENTATION_CONTEXT('','3D')
);
#14347=(
GEOMETRIC_REPRESENTATION_CONTEXT(3)
GLOBAL_UNCERTAINTY_ASSIGNED_CONTEXT((#14299))
GLOBAL_UNIT_ASSIGNED_CONTEXT((#14393,#14395,#14396))
REPRESENTATION_CONTEXT('','3D')
);
#14348=(
GEOMETRIC_REPRESENTATION_CONTEXT(3)
GLOBAL_UNCERTAINTY_ASSIGNED_CONTEXT((#14300))
GLOBAL_UNIT_ASSIGNED_CONTEXT((#14393,#14395,#14396))
REPRESENTATION_CONTEXT('','3D')
);
#14349=(
GEOMETRIC_REPRESENTATION_CONTEXT(3)
GLOBAL_UNCERTAINTY_ASSIGNED_CONTEXT((#14301))
GLOBAL_UNIT_ASSIGNED_CONTEXT((#14393,#14395,#14396))
REPRESENTATION_CONTEXT('','3D')
);
#14350=(
GEOMETRIC_REPRESENTATION_CONTEXT(3)
GLOBAL_UNCERTAINTY_ASSIGNED_CONTEXT((#14302))
GLOBAL_UNIT_ASSIGNED_CONTEXT((#14393,#14395,#14396))
REPRESENTATION_CONTEXT('','3D')
);
#14351=(
GEOMETRIC_REPRESENTATION_CONTEXT(3)
GLOBAL_UNCERTAINTY_ASSIGNED_CONTEXT((#14303))
GLOBAL_UNIT_ASSIGNED_CONTEXT((#14393,#14395,#14396))
REPRESENTATION_CONTEXT('','3D')
);
#14352=(
GEOMETRIC_REPRESENTATION_CONTEXT(3)
GLOBAL_UNCERTAINTY_ASSIGNED_CONTEXT((#14304))
GLOBAL_UNIT_ASSIGNED_CONTEXT((#14393,#14395,#14396))
REPRESENTATION_CONTEXT('','3D')
);
#14353=(
GEOMETRIC_REPRESENTATION_CONTEXT(3)
GLOBAL_UNCERTAINTY_ASSIGNED_CONTEXT((#14305))
GLOBAL_UNIT_ASSIGNED_CONTEXT((#14393,#14395,#14396))
REPRESENTATION_CONTEXT('','3D')
);
#14354=(
GEOMETRIC_REPRESENTATION_CONTEXT(3)
GLOBAL_UNCERTAINTY_ASSIGNED_CONTEXT((#14306))
GLOBAL_UNIT_ASSIGNED_CONTEXT((#14393,#14395,#14396))
REPRESENTATION_CONTEXT('','3D')
);
#14355=(
GEOMETRIC_REPRESENTATION_CONTEXT(3)
GLOBAL_UNCERTAINTY_ASSIGNED_CONTEXT((#14307))
GLOBAL_UNIT_ASSIGNED_CONTEXT((#14393,#14395,#14396))
REPRESENTATION_CONTEXT('','3D')
);
#14356=(
GEOMETRIC_REPRESENTATION_CONTEXT(3)
GLOBAL_UNCERTAINTY_ASSIGNED_CONTEXT((#14308))
GLOBAL_UNIT_ASSIGNED_CONTEXT((#14393,#14395,#14396))
REPRESENTATION_CONTEXT('','3D')
);
#14357=(
GEOMETRIC_REPRESENTATION_CONTEXT(3)
GLOBAL_UNCERTAINTY_ASSIGNED_CONTEXT((#14309))
GLOBAL_UNIT_ASSIGNED_CONTEXT((#14393,#14395,#14396))
REPRESENTATION_CONTEXT('','3D')
);
#14358=(
GEOMETRIC_REPRESENTATION_CONTEXT(3)
GLOBAL_UNCERTAINTY_ASSIGNED_CONTEXT((#14310))
GLOBAL_UNIT_ASSIGNED_CONTEXT((#14393,#14395,#14396))
REPRESENTATION_CONTEXT('','3D')
);
#14359=(
GEOMETRIC_REPRESENTATION_CONTEXT(3)
GLOBAL_UNCERTAINTY_ASSIGNED_CONTEXT((#14311))
GLOBAL_UNIT_ASSIGNED_CONTEXT((#14393,#14395,#14396))
REPRESENTATION_CONTEXT('','3D')
);
#14360=(
GEOMETRIC_REPRESENTATION_CONTEXT(3)
GLOBAL_UNCERTAINTY_ASSIGNED_CONTEXT((#14312))
GLOBAL_UNIT_ASSIGNED_CONTEXT((#14393,#14395,#14396))
REPRESENTATION_CONTEXT('','3D')
);
#14361=(
GEOMETRIC_REPRESENTATION_CONTEXT(3)
GLOBAL_UNCERTAINTY_ASSIGNED_CONTEXT((#14313))
GLOBAL_UNIT_ASSIGNED_CONTEXT((#14393,#14395,#14396))
REPRESENTATION_CONTEXT('','3D')
);
#14362=(
GEOMETRIC_REPRESENTATION_CONTEXT(3)
GLOBAL_UNCERTAINTY_ASSIGNED_CONTEXT((#14314))
GLOBAL_UNIT_ASSIGNED_CONTEXT((#14393,#14395,#14396))
REPRESENTATION_CONTEXT('','3D')
);
#14363=(
GEOMETRIC_REPRESENTATION_CONTEXT(3)
GLOBAL_UNCERTAINTY_ASSIGNED_CONTEXT((#14315))
GLOBAL_UNIT_ASSIGNED_CONTEXT((#14393,#14395,#14396))
REPRESENTATION_CONTEXT('','3D')
);
#14364=(
GEOMETRIC_REPRESENTATION_CONTEXT(3)
GLOBAL_UNCERTAINTY_ASSIGNED_CONTEXT((#14316))
GLOBAL_UNIT_ASSIGNED_CONTEXT((#14393,#14395,#14396))
REPRESENTATION_CONTEXT('','3D')
);
#14365=(
GEOMETRIC_REPRESENTATION_CONTEXT(3)
GLOBAL_UNCERTAINTY_ASSIGNED_CONTEXT((#14317))
GLOBAL_UNIT_ASSIGNED_CONTEXT((#14393,#14395,#14396))
REPRESENTATION_CONTEXT('','3D')
);
#14366=(
GEOMETRIC_REPRESENTATION_CONTEXT(3)
GLOBAL_UNCERTAINTY_ASSIGNED_CONTEXT((#14318))
GLOBAL_UNIT_ASSIGNED_CONTEXT((#14393,#14395,#14396))
REPRESENTATION_CONTEXT('','3D')
);
#14367=(
GEOMETRIC_REPRESENTATION_CONTEXT(3)
GLOBAL_UNCERTAINTY_ASSIGNED_CONTEXT((#14319))
GLOBAL_UNIT_ASSIGNED_CONTEXT((#14393,#14395,#14396))
REPRESENTATION_CONTEXT('','3D')
);
#14368=(
GEOMETRIC_REPRESENTATION_CONTEXT(3)
GLOBAL_UNCERTAINTY_ASSIGNED_CONTEXT((#14320))
GLOBAL_UNIT_ASSIGNED_CONTEXT((#14393,#14395,#14396))
REPRESENTATION_CONTEXT('','3D')
);
#14369=(
GEOMETRIC_REPRESENTATION_CONTEXT(3)
GLOBAL_UNCERTAINTY_ASSIGNED_CONTEXT((#14321))
GLOBAL_UNIT_ASSIGNED_CONTEXT((#14393,#14395,#14396))
REPRESENTATION_CONTEXT('','3D')
);
#14370=(
GEOMETRIC_REPRESENTATION_CONTEXT(3)
GLOBAL_UNCERTAINTY_ASSIGNED_CONTEXT((#14322))
GLOBAL_UNIT_ASSIGNED_CONTEXT((#14393,#14395,#14396))
REPRESENTATION_CONTEXT('','3D')
);
#14371=(
GEOMETRIC_REPRESENTATION_CONTEXT(3)
GLOBAL_UNCERTAINTY_ASSIGNED_CONTEXT((#14323))
GLOBAL_UNIT_ASSIGNED_CONTEXT((#14393,#14395,#14396))
REPRESENTATION_CONTEXT('','3D')
);
#14372=(
GEOMETRIC_REPRESENTATION_CONTEXT(3)
GLOBAL_UNCERTAINTY_ASSIGNED_CONTEXT((#14324))
GLOBAL_UNIT_ASSIGNED_CONTEXT((#14393,#14395,#14396))
REPRESENTATION_CONTEXT('','3D')
);
#14373=(
GEOMETRIC_REPRESENTATION_CONTEXT(3)
GLOBAL_UNCERTAINTY_ASSIGNED_CONTEXT((#14325))
GLOBAL_UNIT_ASSIGNED_CONTEXT((#14393,#14395,#14396))
REPRESENTATION_CONTEXT('','3D')
);
#14374=(
GEOMETRIC_REPRESENTATION_CONTEXT(3)
GLOBAL_UNCERTAINTY_ASSIGNED_CONTEXT((#14326))
GLOBAL_UNIT_ASSIGNED_CONTEXT((#14393,#14395,#14396))
REPRESENTATION_CONTEXT('','3D')
);
#14375=(
GEOMETRIC_REPRESENTATION_CONTEXT(3)
GLOBAL_UNCERTAINTY_ASSIGNED_CONTEXT((#14327))
GLOBAL_UNIT_ASSIGNED_CONTEXT((#14393,#14395,#14396))
REPRESENTATION_CONTEXT('','3D')
);
#14376=(
GEOMETRIC_REPRESENTATION_CONTEXT(3)
GLOBAL_UNCERTAINTY_ASSIGNED_CONTEXT((#14328))
GLOBAL_UNIT_ASSIGNED_CONTEXT((#14393,#14395,#14396))
REPRESENTATION_CONTEXT('','3D')
);
#14377=(
GEOMETRIC_REPRESENTATION_CONTEXT(3)
GLOBAL_UNCERTAINTY_ASSIGNED_CONTEXT((#14329))
GLOBAL_UNIT_ASSIGNED_CONTEXT((#14393,#14395,#14396))
REPRESENTATION_CONTEXT('','3D')
);
#14378=(
GEOMETRIC_REPRESENTATION_CONTEXT(3)
GLOBAL_UNCERTAINTY_ASSIGNED_CONTEXT((#14330))
GLOBAL_UNIT_ASSIGNED_CONTEXT((#14393,#14395,#14396))
REPRESENTATION_CONTEXT('','3D')
);
#14379=(
GEOMETRIC_REPRESENTATION_CONTEXT(3)
GLOBAL_UNCERTAINTY_ASSIGNED_CONTEXT((#14331))
GLOBAL_UNIT_ASSIGNED_CONTEXT((#14393,#14395,#14396))
REPRESENTATION_CONTEXT('','3D')
);
#14380=(
GEOMETRIC_REPRESENTATION_CONTEXT(3)
GLOBAL_UNCERTAINTY_ASSIGNED_CONTEXT((#14332))
GLOBAL_UNIT_ASSIGNED_CONTEXT((#14393,#14395,#14396))
REPRESENTATION_CONTEXT('','3D')
);
#14381=(
GEOMETRIC_REPRESENTATION_CONTEXT(3)
GLOBAL_UNCERTAINTY_ASSIGNED_CONTEXT((#14333))
GLOBAL_UNIT_ASSIGNED_CONTEXT((#14393,#14395,#14396))
REPRESENTATION_CONTEXT('','3D')
);
#14382=(
GEOMETRIC_REPRESENTATION_CONTEXT(3)
GLOBAL_UNCERTAINTY_ASSIGNED_CONTEXT((#14334))
GLOBAL_UNIT_ASSIGNED_CONTEXT((#14393,#14395,#14396))
REPRESENTATION_CONTEXT('','3D')
);
#14383=(
GEOMETRIC_REPRESENTATION_CONTEXT(3)
GLOBAL_UNCERTAINTY_ASSIGNED_CONTEXT((#14335))
GLOBAL_UNIT_ASSIGNED_CONTEXT((#14393,#14395,#14396))
REPRESENTATION_CONTEXT('','3D')
);
#14384=(
GEOMETRIC_REPRESENTATION_CONTEXT(3)
GLOBAL_UNCERTAINTY_ASSIGNED_CONTEXT((#14336))
GLOBAL_UNIT_ASSIGNED_CONTEXT((#14393,#14395,#14396))
REPRESENTATION_CONTEXT('','3D')
);
#14385=(
GEOMETRIC_REPRESENTATION_CONTEXT(3)
GLOBAL_UNCERTAINTY_ASSIGNED_CONTEXT((#14337))
GLOBAL_UNIT_ASSIGNED_CONTEXT((#14393,#14395,#14396))
REPRESENTATION_CONTEXT('','3D')
);
#14386=(
GEOMETRIC_REPRESENTATION_CONTEXT(3)
GLOBAL_UNCERTAINTY_ASSIGNED_CONTEXT((#14338))
GLOBAL_UNIT_ASSIGNED_CONTEXT((#14393,#14395,#14396))
REPRESENTATION_CONTEXT('','3D')
);
#14387=(
GEOMETRIC_REPRESENTATION_CONTEXT(3)
GLOBAL_UNCERTAINTY_ASSIGNED_CONTEXT((#14339))
GLOBAL_UNIT_ASSIGNED_CONTEXT((#14393,#14395,#14396))
REPRESENTATION_CONTEXT('','3D')
);
#14388=(
GEOMETRIC_REPRESENTATION_CONTEXT(3)
GLOBAL_UNCERTAINTY_ASSIGNED_CONTEXT((#14340))
GLOBAL_UNIT_ASSIGNED_CONTEXT((#14393,#14395,#14396))
REPRESENTATION_CONTEXT('','3D')
);
#14389=(
GEOMETRIC_REPRESENTATION_CONTEXT(3)
GLOBAL_UNCERTAINTY_ASSIGNED_CONTEXT((#14341))
GLOBAL_UNIT_ASSIGNED_CONTEXT((#14393,#14395,#14396))
REPRESENTATION_CONTEXT('','3D')
);
#14390=(
GEOMETRIC_REPRESENTATION_CONTEXT(3)
GLOBAL_UNCERTAINTY_ASSIGNED_CONTEXT((#14342))
GLOBAL_UNIT_ASSIGNED_CONTEXT((#14393,#14395,#14396))
REPRESENTATION_CONTEXT('','3D')
);
#14391=(
GEOMETRIC_REPRESENTATION_CONTEXT(3)
GLOBAL_UNCERTAINTY_ASSIGNED_CONTEXT((#14343))
GLOBAL_UNIT_ASSIGNED_CONTEXT((#14393,#14395,#14396))
REPRESENTATION_CONTEXT('','3D')
);
#14392=(
GEOMETRIC_REPRESENTATION_CONTEXT(3)
GLOBAL_UNCERTAINTY_ASSIGNED_CONTEXT((#14344))
GLOBAL_UNIT_ASSIGNED_CONTEXT((#14393,#14395,#14396))
REPRESENTATION_CONTEXT('','3D')
);
#14393=(
LENGTH_UNIT()
NAMED_UNIT(*)
SI_UNIT(.CENTI.,.METRE.)
);
#14394=(
LENGTH_UNIT()
NAMED_UNIT(*)
SI_UNIT($,.METRE.)
);
#14395=(
NAMED_UNIT(*)
PLANE_ANGLE_UNIT()
SI_UNIT($,.RADIAN.)
);
#14396=(
NAMED_UNIT(*)
SI_UNIT($,.STERADIAN.)
SOLID_ANGLE_UNIT()
);
#14397=SHAPE_DEFINITION_REPRESENTATION(#14444,#14583);
#14398=SHAPE_DEFINITION_REPRESENTATION(#14445,#14584);
#14399=SHAPE_DEFINITION_REPRESENTATION(#14446,#14585);
#14400=SHAPE_DEFINITION_REPRESENTATION(#14447,#14586);
#14401=SHAPE_DEFINITION_REPRESENTATION(#14448,#14587);
#14402=SHAPE_DEFINITION_REPRESENTATION(#14449,#14588);
#14403=SHAPE_DEFINITION_REPRESENTATION(#14450,#14589);
#14404=SHAPE_DEFINITION_REPRESENTATION(#14451,#14590);
#14405=SHAPE_DEFINITION_REPRESENTATION(#14452,#14591);
#14406=SHAPE_DEFINITION_REPRESENTATION(#14453,#14592);
#14407=SHAPE_DEFINITION_REPRESENTATION(#14454,#14593);
#14408=SHAPE_DEFINITION_REPRESENTATION(#14455,#14594);
#14409=SHAPE_DEFINITION_REPRESENTATION(#14456,#14595);
#14410=SHAPE_DEFINITION_REPRESENTATION(#14457,#14596);
#14411=SHAPE_DEFINITION_REPRESENTATION(#14458,#14597);
#14412=SHAPE_DEFINITION_REPRESENTATION(#14459,#14598);
#14413=SHAPE_DEFINITION_REPRESENTATION(#14462,#14599);
#14414=SHAPE_DEFINITION_REPRESENTATION(#14463,#14600);
#14415=SHAPE_DEFINITION_REPRESENTATION(#14464,#14601);
#14416=SHAPE_DEFINITION_REPRESENTATION(#14465,#14602);
#14417=SHAPE_DEFINITION_REPRESENTATION(#14466,#14603);
#14418=SHAPE_DEFINITION_REPRESENTATION(#14467,#14604);
#14419=SHAPE_DEFINITION_REPRESENTATION(#14468,#14605);
#14420=SHAPE_DEFINITION_REPRESENTATION(#14469,#14606);
#14421=SHAPE_DEFINITION_REPRESENTATION(#14470,#14607);
#14422=SHAPE_DEFINITION_REPRESENTATION(#14471,#14608);
#14423=SHAPE_DEFINITION_REPRESENTATION(#14472,#14609);
#14424=SHAPE_DEFINITION_REPRESENTATION(#14473,#14610);
#14425=SHAPE_DEFINITION_REPRESENTATION(#14474,#14611);
#14426=SHAPE_DEFINITION_REPRESENTATION(#14475,#14612);
#14427=SHAPE_DEFINITION_REPRESENTATION(#14478,#14613);
#14428=SHAPE_DEFINITION_REPRESENTATION(#14479,#14614);
#14429=SHAPE_DEFINITION_REPRESENTATION(#14548,#14615);
#14430=SHAPE_DEFINITION_REPRESENTATION(#14549,#14616);
#14431=SHAPE_DEFINITION_REPRESENTATION(#14550,#14617);
#14432=SHAPE_DEFINITION_REPRESENTATION(#14551,#14618);
#14433=SHAPE_DEFINITION_REPRESENTATION(#14552,#14619);
#14434=SHAPE_DEFINITION_REPRESENTATION(#14553,#14620);
#14435=SHAPE_DEFINITION_REPRESENTATION(#14554,#14621);
#14436=SHAPE_DEFINITION_REPRESENTATION(#14555,#14622);
#14437=SHAPE_DEFINITION_REPRESENTATION(#14556,#14623);
#14438=SHAPE_DEFINITION_REPRESENTATION(#14557,#14624);
#14439=SHAPE_DEFINITION_REPRESENTATION(#14558,#14625);
#14440=SHAPE_DEFINITION_REPRESENTATION(#14559,#14626);
#14441=SHAPE_DEFINITION_REPRESENTATION(#14560,#14627);
#14442=SHAPE_DEFINITION_REPRESENTATION(#14561,#14628);
#14443=SHAPE_DEFINITION_REPRESENTATION(#14562,#14629);
#14444=PRODUCT_DEFINITION_SHAPE('',$,#14631);
#14445=PRODUCT_DEFINITION_SHAPE('',$,#14632);
#14446=PRODUCT_DEFINITION_SHAPE('',$,#14633);
#14447=PRODUCT_DEFINITION_SHAPE('',$,#14634);
#14448=PRODUCT_DEFINITION_SHAPE('',$,#14635);
#14449=PRODUCT_DEFINITION_SHAPE('',$,#14636);
#14450=PRODUCT_DEFINITION_SHAPE('',$,#14637);
#14451=PRODUCT_DEFINITION_SHAPE('',$,#14638);
#14452=PRODUCT_DEFINITION_SHAPE('',$,#14639);
#14453=PRODUCT_DEFINITION_SHAPE('',$,#14640);
#14454=PRODUCT_DEFINITION_SHAPE('',$,#14641);
#14455=PRODUCT_DEFINITION_SHAPE('',$,#14642);
#14456=PRODUCT_DEFINITION_SHAPE('',$,#14643);
#14457=PRODUCT_DEFINITION_SHAPE('',$,#14644);
#14458=PRODUCT_DEFINITION_SHAPE('',$,#14645);
#14459=PRODUCT_DEFINITION_SHAPE('',$,#14646);
#14460=PRODUCT_DEFINITION_SHAPE($,$,#323);
#14461=PRODUCT_DEFINITION_SHAPE($,$,#324);
#14462=PRODUCT_DEFINITION_SHAPE('',$,#14647);
#14463=PRODUCT_DEFINITION_SHAPE('',$,#14648);
#14464=PRODUCT_DEFINITION_SHAPE('',$,#14649);
#14465=PRODUCT_DEFINITION_SHAPE('',$,#14650);
#14466=PRODUCT_DEFINITION_SHAPE('',$,#14651);
#14467=PRODUCT_DEFINITION_SHAPE('',$,#14652);
#14468=PRODUCT_DEFINITION_SHAPE('',$,#14653);
#14469=PRODUCT_DEFINITION_SHAPE('',$,#14654);
#14470=PRODUCT_DEFINITION_SHAPE('',$,#14655);
#14471=PRODUCT_DEFINITION_SHAPE('',$,#14656);
#14472=PRODUCT_DEFINITION_SHAPE('',$,#14657);
#14473=PRODUCT_DEFINITION_SHAPE('',$,#14658);
#14474=PRODUCT_DEFINITION_SHAPE('',$,#14659);
#14475=PRODUCT_DEFINITION_SHAPE('',$,#14660);
#14476=PRODUCT_DEFINITION_SHAPE($,$,#325);
#14477=PRODUCT_DEFINITION_SHAPE($,$,#326);
#14478=PRODUCT_DEFINITION_SHAPE('',$,#14661);
#14479=PRODUCT_DEFINITION_SHAPE('',$,#14662);
#14480=PRODUCT_DEFINITION_SHAPE($,$,#327);
#14481=PRODUCT_DEFINITION_SHAPE($,$,#328);
#14482=PRODUCT_DEFINITION_SHAPE($,$,#329);
#14483=PRODUCT_DEFINITION_SHAPE($,$,#330);
#14484=PRODUCT_DEFINITION_SHAPE($,$,#331);
#14485=PRODUCT_DEFINITION_SHAPE($,$,#332);
#14486=PRODUCT_DEFINITION_SHAPE($,$,#333);
#14487=PRODUCT_DEFINITION_SHAPE($,$,#334);
#14488=PRODUCT_DEFINITION_SHAPE($,$,#335);
#14489=PRODUCT_DEFINITION_SHAPE($,$,#336);
#14490=PRODUCT_DEFINITION_SHAPE($,$,#337);
#14491=PRODUCT_DEFINITION_SHAPE($,$,#338);
#14492=PRODUCT_DEFINITION_SHAPE($,$,#339);
#14493=PRODUCT_DEFINITION_SHAPE($,$,#340);
#14494=PRODUCT_DEFINITION_SHAPE($,$,#341);
#14495=PRODUCT_DEFINITION_SHAPE($,$,#342);
#14496=PRODUCT_DEFINITION_SHAPE($,$,#343);
#14497=PRODUCT_DEFINITION_SHAPE($,$,#344);
#14498=PRODUCT_DEFINITION_SHAPE($,$,#345);
#14499=PRODUCT_DEFINITION_SHAPE($,$,#346);
#14500=PRODUCT_DEFINITION_SHAPE($,$,#347);
#14501=PRODUCT_DEFINITION_SHAPE($,$,#348);
#14502=PRODUCT_DEFINITION_SHAPE($,$,#349);
#14503=PRODUCT_DEFINITION_SHAPE($,$,#350);
#14504=PRODUCT_DEFINITION_SHAPE($,$,#351);
#14505=PRODUCT_DEFINITION_SHAPE($,$,#352);
#14506=PRODUCT_DEFINITION_SHAPE($,$,#353);
#14507=PRODUCT_DEFINITION_SHAPE($,$,#354);
#14508=PRODUCT_DEFINITION_SHAPE($,$,#355);
#14509=PRODUCT_DEFINITION_SHAPE($,$,#356);
#14510=PRODUCT_DEFINITION_SHAPE($,$,#357);
#14511=PRODUCT_DEFINITION_SHAPE($,$,#358);
#14512=PRODUCT_DEFINITION_SHAPE($,$,#359);
#14513=PRODUCT_DEFINITION_SHAPE($,$,#360);
#14514=PRODUCT_DEFINITION_SHAPE($,$,#361);
#14515=PRODUCT_DEFINITION_SHAPE($,$,#362);
#14516=PRODUCT_DEFINITION_SHAPE($,$,#363);
#14517=PRODUCT_DEFINITION_SHAPE($,$,#364);
#14518=PRODUCT_DEFINITION_SHAPE($,$,#365);
#14519=PRODUCT_DEFINITION_SHAPE($,$,#366);
#14520=PRODUCT_DEFINITION_SHAPE($,$,#367);
#14521=PRODUCT_DEFINITION_SHAPE($,$,#368);
#14522=PRODUCT_DEFINITION_SHAPE($,$,#369);
#14523=PRODUCT_DEFINITION_SHAPE($,$,#370);
#14524=PRODUCT_DEFINITION_SHAPE($,$,#371);
#14525=PRODUCT_DEFINITION_SHAPE($,$,#372);
#14526=PRODUCT_DEFINITION_SHAPE($,$,#373);
#14527=PRODUCT_DEFINITION_SHAPE($,$,#374);
#14528=PRODUCT_DEFINITION_SHAPE($,$,#375);
#14529=PRODUCT_DEFINITION_SHAPE($,$,#376);
#14530=PRODUCT_DEFINITION_SHAPE($,$,#377);
#14531=PRODUCT_DEFINITION_SHAPE($,$,#378);
#14532=PRODUCT_DEFINITION_SHAPE($,$,#379);
#14533=PRODUCT_DEFINITION_SHAPE($,$,#380);
#14534=PRODUCT_DEFINITION_SHAPE($,$,#381);
#14535=PRODUCT_DEFINITION_SHAPE($,$,#382);
#14536=PRODUCT_DEFINITION_SHAPE($,$,#383);
#14537=PRODUCT_DEFINITION_SHAPE($,$,#384);
#14538=PRODUCT_DEFINITION_SHAPE($,$,#385);
#14539=PRODUCT_DEFINITION_SHAPE($,$,#386);
#14540=PRODUCT_DEFINITION_SHAPE($,$,#387);
#14541=PRODUCT_DEFINITION_SHAPE($,$,#388);
#14542=PRODUCT_DEFINITION_SHAPE($,$,#389);
#14543=PRODUCT_DEFINITION_SHAPE($,$,#390);
#14544=PRODUCT_DEFINITION_SHAPE($,$,#391);
#14545=PRODUCT_DEFINITION_SHAPE($,$,#392);
#14546=PRODUCT_DEFINITION_SHAPE($,$,#393);
#14547=PRODUCT_DEFINITION_SHAPE($,$,#394);
#14548=PRODUCT_DEFINITION_SHAPE('',$,#14663);
#14549=PRODUCT_DEFINITION_SHAPE('',$,#14664);
#14550=PRODUCT_DEFINITION_SHAPE('',$,#14665);
#14551=PRODUCT_DEFINITION_SHAPE('',$,#14666);
#14552=PRODUCT_DEFINITION_SHAPE('',$,#14667);
#14553=PRODUCT_DEFINITION_SHAPE('',$,#14668);
#14554=PRODUCT_DEFINITION_SHAPE('',$,#14669);
#14555=PRODUCT_DEFINITION_SHAPE('',$,#14670);
#14556=PRODUCT_DEFINITION_SHAPE('',$,#14671);
#14557=PRODUCT_DEFINITION_SHAPE('',$,#14672);
#14558=PRODUCT_DEFINITION_SHAPE('',$,#14673);
#14559=PRODUCT_DEFINITION_SHAPE('',$,#14674);
#14560=PRODUCT_DEFINITION_SHAPE('',$,#14675);
#14561=PRODUCT_DEFINITION_SHAPE('',$,#14676);
#14562=PRODUCT_DEFINITION_SHAPE('',$,#14677);
#14563=PRODUCT_DEFINITION_SHAPE($,$,#395);
#14564=PRODUCT_DEFINITION_SHAPE($,$,#396);
#14565=PRODUCT_DEFINITION_SHAPE($,$,#397);
#14566=PRODUCT_DEFINITION_SHAPE($,$,#398);
#14567=PRODUCT_DEFINITION_SHAPE($,$,#399);
#14568=PRODUCT_DEFINITION_SHAPE($,$,#400);
#14569=PRODUCT_DEFINITION_SHAPE($,$,#401);
#14570=PRODUCT_DEFINITION_SHAPE($,$,#402);
#14571=PRODUCT_DEFINITION_SHAPE($,$,#403);
#14572=PRODUCT_DEFINITION_SHAPE($,$,#404);
#14573=PRODUCT_DEFINITION_SHAPE($,$,#405);
#14574=PRODUCT_DEFINITION_SHAPE($,$,#406);
#14575=PRODUCT_DEFINITION_SHAPE($,$,#407);
#14576=PRODUCT_DEFINITION_SHAPE($,$,#408);
#14577=PRODUCT_DEFINITION_SHAPE($,$,#409);
#14578=PRODUCT_DEFINITION_SHAPE($,$,#410);
#14579=PRODUCT_DEFINITION_SHAPE($,$,#411);
#14580=PRODUCT_DEFINITION_SHAPE($,$,#412);
#14581=PRODUCT_DEFINITION_SHAPE($,$,#413);
#14582=PRODUCT_DEFINITION_SHAPE($,$,#414);
#14583=SHAPE_REPRESENTATION('',(#8384,#9379,#9380),#14345);
#14584=SHAPE_REPRESENTATION('',(#8385,#9086,#9087,#9088,#9089,#9090,#9091,
#9092,#9093,#9094,#9095,#9096,#9097,#9098,#9099,#9100,#9101,#9102,#9103,
#9104,#9105,#9106,#9107,#9108,#9109,#9110,#9111,#9112,#9113,#9114,#9115,
#9116,#9117,#9118,#9119,#9120,#9121,#9122,#9123,#9124,#9125,#9126,#9127,
#9128,#9129,#9130,#9131,#9132,#9133,#9134,#9135,#9136,#9137,#9138,#9139,
#9140,#9141,#9142,#9143,#9144,#9145,#9146,#9147,#9148,#9149,#9150,#9151,
#9152,#9153),#14346);
#14585=SHAPE_REPRESENTATION('',(#8386),#14347);
#14586=SHAPE_REPRESENTATION('',(#8456),#14348);
#14587=SHAPE_REPRESENTATION('',(#8500),#14349);
#14588=SHAPE_REPRESENTATION('',(#8512),#14350);
#14589=SHAPE_REPRESENTATION('',(#8579),#14351);
#14590=SHAPE_REPRESENTATION('',(#8623),#14352);
#14591=SHAPE_REPRESENTATION('',(#8635),#14353);
#14592=SHAPE_REPRESENTATION('',(#8644),#14354);
#14593=SHAPE_REPRESENTATION('',(#8653),#14355);
#14594=SHAPE_REPRESENTATION('',(#8662),#14356);
#14595=SHAPE_REPRESENTATION('',(#8697),#14357);
#14596=SHAPE_REPRESENTATION('',(#8723,#8765,#8766),#14358);
#14597=SHAPE_REPRESENTATION('',(#8724),#14359);
#14598=SHAPE_REPRESENTATION('',(#8752),#14360);
#14599=SHAPE_REPRESENTATION('',(#8767),#14361);
#14600=SHAPE_REPRESENTATION('',(#8771),#14362);
#14601=SHAPE_REPRESENTATION('',(#8788),#14363);
#14602=SHAPE_REPRESENTATION('',(#8792),#14364);
#14603=SHAPE_REPRESENTATION('',(#8798),#14365);
#14604=SHAPE_REPRESENTATION('',(#8809),#14366);
#14605=SHAPE_REPRESENTATION('',(#8825),#14367);
#14606=SHAPE_REPRESENTATION('',(#8896),#14368);
#14607=SHAPE_REPRESENTATION('',(#8917),#14369);
#14608=SHAPE_REPRESENTATION('',(#8938),#14370);
#14609=SHAPE_REPRESENTATION('',(#8959),#14371);
#14610=SHAPE_REPRESENTATION('',(#8980,#9030,#9031),#14372);
#14611=SHAPE_REPRESENTATION('',(#8981),#14373);
#14612=SHAPE_REPRESENTATION('',(#9013),#14374);
#14613=SHAPE_REPRESENTATION('',(#9032),#14375);
#14614=SHAPE_REPRESENTATION('',(#9056),#14376);
#14615=SHAPE_REPRESENTATION('',(#9154,#9361,#9362,#9363,#9364,#9365,#9366,
#9367,#9368,#9369,#9370,#9371,#9372,#9373,#9374,#9375,#9376,#9377,#9378),
#14377);
#14616=SHAPE_REPRESENTATION('',(#9155),#14378);
#14617=SHAPE_REPRESENTATION('',(#9176),#14379);
#14618=SHAPE_REPRESENTATION('',(#9180),#14380);
#14619=SHAPE_REPRESENTATION('',(#9190),#14381);
#14620=SHAPE_REPRESENTATION('',(#9216),#14382);
#14621=SHAPE_REPRESENTATION('',(#9243),#14383);
#14622=SHAPE_REPRESENTATION('',(#9260),#14384);
#14623=SHAPE_REPRESENTATION('',(#9275),#14385);
#14624=SHAPE_REPRESENTATION('',(#9284),#14386);
#14625=SHAPE_REPRESENTATION('',(#9295),#14387);
#14626=SHAPE_REPRESENTATION('',(#9305),#14388);
#14627=SHAPE_REPRESENTATION('',(#9315),#14389);
#14628=SHAPE_REPRESENTATION('',(#9336),#14390);
#14629=SHAPE_REPRESENTATION('',(#9345),#14391);
#14630=PRODUCT_DEFINITION_CONTEXT('part definition',#14773,'design');
#14631=PRODUCT_DEFINITION('PAT-048','PAT-048',#14678,
#14630);
#14632=PRODUCT_DEFINITION(
'Twenty millimetre bore cylinder and flow controls',
'Twenty millimetre bore cylinder and flow controls',#14679,#14630);
#14633=PRODUCT_DEFINITION('Front cylinder cap','Front cylinder cap',#14680,
#14630);
#14634=PRODUCT_DEFINITION('Needle flow-control fitting',
'Needle flow-control fitting',#14681,#14630);
#14635=PRODUCT_DEFINITION('Metering needle and grip',
'Metering needle and grip',#14682,#14630);
#14636=PRODUCT_DEFINITION('Rear cylinder cap','Rear cylinder cap',#14683,
#14630);
#14637=PRODUCT_DEFINITION('Needle flow-control fitting (1)',
'Needle flow-control fitting (1)',#14684,#14630);
#14638=PRODUCT_DEFINITION('Metering needle and grip (1)',
'Metering needle and grip (1)',#14685,#14630);
#14639=PRODUCT_DEFINITION('Twenty millimetre bore barrel',
'Twenty millimetre bore barrel',#14686,#14630);
#14640=PRODUCT_DEFINITION('Barrel end gasket','Barrel end gasket',#14687,
#14630);
#14641=PRODUCT_DEFINITION('Barrel end gasket (1)','Barrel end gasket (1)',
#14688,#14630);
#14642=PRODUCT_DEFINITION('Recessed cylinder mounting foot',
'Recessed cylinder mounting foot',#14689,#14630);
#14643=PRODUCT_DEFINITION('Cap Screw - M5x20','Cap Screw - M5x20',#14690,
#14630);
#14644=PRODUCT_DEFINITION(
'Push-In Tube Fitting - 6 mm Tube, 1-8 Inch Tapered Pipe Thread',
'Push-In Tube Fitting - 6 mm Tube, 1-8 Inch Tapered Pipe Thread',#14691,
#14630);
#14645=PRODUCT_DEFINITION('Body','Body',#14692,#14630);
#14646=PRODUCT_DEFINITION('Release collar','Release collar',#14693,#14630);
#14647=PRODUCT_DEFINITION('O-Ring','O-Ring',#14694,#14630);
#14648=PRODUCT_DEFINITION('Rod guide','Rod guide',#14695,#14630);
#14649=PRODUCT_DEFINITION('Rod seal','Rod seal',#14696,#14630);
#14650=PRODUCT_DEFINITION('M5 tie rod','M5 tie rod',#14697,#14630);
#14651=PRODUCT_DEFINITION('Flat Washer - M5','Flat Washer - M5',#14698,
#14630);
#14652=PRODUCT_DEFINITION('Hex Nut - M5','Hex Nut - M5',#14699,#14630);
#14653=PRODUCT_DEFINITION('Cylinder and guide mounting frame',
'Cylinder and guide mounting frame',#14700,#14630);
#14654=PRODUCT_DEFINITION('Linear bearing retaining cap',
'Linear bearing retaining cap',#14701,#14630);
#14655=PRODUCT_DEFINITION('Linear bearing retaining cap (1)',
'Linear bearing retaining cap (1)',#14702,#14630);
#14656=PRODUCT_DEFINITION('Linear bearing retaining cap (2)',
'Linear bearing retaining cap (2)',#14703,#14630);
#14657=PRODUCT_DEFINITION('Linear bearing retaining cap (3)',
'Linear bearing retaining cap (3)',#14704,#14630);
#14658=PRODUCT_DEFINITION('Linear Ball Bushing - 12 x 21 x 30 mm',
'Linear Ball Bushing - 12 x 21 x 30 mm',#14705,#14630);
#14659=PRODUCT_DEFINITION('Steel sleeve','Steel sleeve',#14706,#14630);
#14660=PRODUCT_DEFINITION('Ball retainer (plastic)',
'Ball retainer (plastic)',#14707,#14630);
#14661=PRODUCT_DEFINITION('M4x10 Cap Screw','M4x10 Cap Screw',#14708,#14630);
#14662=PRODUCT_DEFINITION('Cylinder foot screw','Cylinder foot screw',#14709,
#14630);
#14663=PRODUCT_DEFINITION('Piston rod and clevis',
'Piston rod and clevis',#14710,#14630);
#14664=PRODUCT_DEFINITION('Twenty millimetre piston',
'Twenty millimetre piston',#14711,#14630);
#14665=PRODUCT_DEFINITION('Piston seal','Piston seal',#14712,#14630);
#14666=PRODUCT_DEFINITION('Piston rod','Piston rod',#14713,#14630);
#14667=PRODUCT_DEFINITION('Cap Screw - M4x16','Cap Screw - M4x16',#14714,
#14630);
#14668=PRODUCT_DEFINITION('Six-millimetre-pin rod clevis',
'Six-millimetre-pin rod clevis',#14715,#14630);
#14669=PRODUCT_DEFINITION('Socket Set Screw - M4x6',
'Socket Set Screw - M4x6',#14716,#14630);
#14670=PRODUCT_DEFINITION('Clevis Pin - 6x30','Clevis Pin - 6x30',#14717,
#14630);
#14671=PRODUCT_DEFINITION('Flat Washer - M6','Flat Washer - M6',#14718,
#14630);
#14672=PRODUCT_DEFINITION('Split Pin - 1.6x16','Split Pin - 1.6x16',#14719,
#14630);
#14673=PRODUCT_DEFINITION('Stepped guide rod','Stepped guide rod',#14720,
#14630);
#14674=PRODUCT_DEFINITION('Stepped guide rod (1)','Stepped guide rod (1)',
#14721,#14630);
#14675=PRODUCT_DEFINITION('Product stop crosshead',
'Product stop crosshead',#14722,#14630);
#14676=PRODUCT_DEFINITION('Flat Washer - M6 (1)','Flat Washer - M6 (1)',#14723,
#14630);
#14677=PRODUCT_DEFINITION('Hex Nut - M6','Hex Nut - M6',#14724,#14630);
#14678=PRODUCT_DEFINITION_FORMATION('',$,#14775);
#14679=PRODUCT_DEFINITION_FORMATION('',$,#14776);
#14680=PRODUCT_DEFINITION_FORMATION('',$,#14777);
#14681=PRODUCT_DEFINITION_FORMATION('',$,#14778);
#14682=PRODUCT_DEFINITION_FORMATION('',$,#14779);
#14683=PRODUCT_DEFINITION_FORMATION('',$,#14780);
#14684=PRODUCT_DEFINITION_FORMATION('',$,#14781);
#14685=PRODUCT_DEFINITION_FORMATION('',$,#14782);
#14686=PRODUCT_DEFINITION_FORMATION('',$,#14783);
#14687=PRODUCT_DEFINITION_FORMATION('',$,#14784);
#14688=PRODUCT_DEFINITION_FORMATION('',$,#14785);
#14689=PRODUCT_DEFINITION_FORMATION('',$,#14786);
#14690=PRODUCT_DEFINITION_FORMATION('',$,#14787);
#14691=PRODUCT_DEFINITION_FORMATION('',$,#14788);
#14692=PRODUCT_DEFINITION_FORMATION('',$,#14789);
#14693=PRODUCT_DEFINITION_FORMATION('',$,#14790);
#14694=PRODUCT_DEFINITION_FORMATION('',$,#14791);
#14695=PRODUCT_DEFINITION_FORMATION('',$,#14792);
#14696=PRODUCT_DEFINITION_FORMATION('',$,#14793);
#14697=PRODUCT_DEFINITION_FORMATION('',$,#14794);
#14698=PRODUCT_DEFINITION_FORMATION('',$,#14795);
#14699=PRODUCT_DEFINITION_FORMATION('',$,#14796);
#14700=PRODUCT_DEFINITION_FORMATION('',$,#14797);
#14701=PRODUCT_DEFINITION_FORMATION('',$,#14798);
#14702=PRODUCT_DEFINITION_FORMATION('',$,#14799);
#14703=PRODUCT_DEFINITION_FORMATION('',$,#14800);
#14704=PRODUCT_DEFINITION_FORMATION('',$,#14801);
#14705=PRODUCT_DEFINITION_FORMATION('',$,#14802);
#14706=PRODUCT_DEFINITION_FORMATION('',$,#14803);
#14707=PRODUCT_DEFINITION_FORMATION('',$,#14804);
#14708=PRODUCT_DEFINITION_FORMATION('',$,#14805);
#14709=PRODUCT_DEFINITION_FORMATION('',$,#14806);
#14710=PRODUCT_DEFINITION_FORMATION('',$,#14807);
#14711=PRODUCT_DEFINITION_FORMATION('',$,#14808);
#14712=PRODUCT_DEFINITION_FORMATION('',$,#14809);
#14713=PRODUCT_DEFINITION_FORMATION('',$,#14810);
#14714=PRODUCT_DEFINITION_FORMATION('',$,#14811);
#14715=PRODUCT_DEFINITION_FORMATION('',$,#14812);
#14716=PRODUCT_DEFINITION_FORMATION('',$,#14813);
#14717=PRODUCT_DEFINITION_FORMATION('',$,#14814);
#14718=PRODUCT_DEFINITION_FORMATION('',$,#14815);
#14719=PRODUCT_DEFINITION_FORMATION('',$,#14816);
#14720=PRODUCT_DEFINITION_FORMATION('',$,#14817);
#14721=PRODUCT_DEFINITION_FORMATION('',$,#14818);
#14722=PRODUCT_DEFINITION_FORMATION('',$,#14819);
#14723=PRODUCT_DEFINITION_FORMATION('',$,#14820);
#14724=PRODUCT_DEFINITION_FORMATION('',$,#14821);
#14725=PRODUCT_RELATED_PRODUCT_CATEGORY('PAT-048','PAT-048',(#14775));
#14726=PRODUCT_RELATED_PRODUCT_CATEGORY(
'Twenty millimetre bore cylinder and flow controls',
'Twenty millimetre bore cylinder and flow controls',(#14776));
#14727=PRODUCT_RELATED_PRODUCT_CATEGORY('Front cylinder cap',
'Front cylinder cap',(#14777));
#14728=PRODUCT_RELATED_PRODUCT_CATEGORY('Needle flow-control fitting',
'Needle flow-control fitting',(#14778));
#14729=PRODUCT_RELATED_PRODUCT_CATEGORY('Metering needle and grip',
'Metering needle and grip',(#14779));
#14730=PRODUCT_RELATED_PRODUCT_CATEGORY('Rear cylinder cap',
'Rear cylinder cap',(#14780));
#14731=PRODUCT_RELATED_PRODUCT_CATEGORY(
'Needle flow-control fitting (1)','Needle flow-control fitting (1)',(#14781));
#14732=PRODUCT_RELATED_PRODUCT_CATEGORY('Metering needle and grip (1)',
'Metering needle and grip (1)',(#14782));
#14733=PRODUCT_RELATED_PRODUCT_CATEGORY('Twenty millimetre bore barrel',
'Twenty millimetre bore barrel',(#14783));
#14734=PRODUCT_RELATED_PRODUCT_CATEGORY('Barrel end gasket',
'Barrel end gasket',(#14784));
#14735=PRODUCT_RELATED_PRODUCT_CATEGORY('Barrel end gasket (1)',
'Barrel end gasket (1)',(#14785));
#14736=PRODUCT_RELATED_PRODUCT_CATEGORY(
'Recessed cylinder mounting foot','Recessed cylinder mounting foot',(#14786));
#14737=PRODUCT_RELATED_PRODUCT_CATEGORY('Cap Screw - M5x20',
'Cap Screw - M5x20',(#14787));
#14738=PRODUCT_RELATED_PRODUCT_CATEGORY(
'Push-In Tube Fitting - 6 mm Tube, 1-8 Inch Tapered Pipe Thread',
'Push-In Tube Fitting - 6 mm Tube, 1-8 Inch Tapered Pipe Thread',(#14788));
#14739=PRODUCT_RELATED_PRODUCT_CATEGORY('Body','Body',(#14789));
#14740=PRODUCT_RELATED_PRODUCT_CATEGORY('Release collar',
'Release collar',(#14790));
#14741=PRODUCT_RELATED_PRODUCT_CATEGORY('O-Ring','O-Ring',(#14791));
#14742=PRODUCT_RELATED_PRODUCT_CATEGORY('Rod guide','Rod guide',(#14792));
#14743=PRODUCT_RELATED_PRODUCT_CATEGORY('Rod seal','Rod seal',(#14793));
#14744=PRODUCT_RELATED_PRODUCT_CATEGORY('M5 tie rod','M5 tie rod',(#14794));
#14745=PRODUCT_RELATED_PRODUCT_CATEGORY('Flat Washer - M5',
'Flat Washer - M5',(#14795));
#14746=PRODUCT_RELATED_PRODUCT_CATEGORY('Hex Nut - M5','Hex Nut - M5',(#14796));
#14747=PRODUCT_RELATED_PRODUCT_CATEGORY(
'Cylinder and guide mounting frame','Cylinder and guide mounting frame',
(#14797));
#14748=PRODUCT_RELATED_PRODUCT_CATEGORY('Linear bearing retaining cap',
'Linear bearing retaining cap',(#14798));
#14749=PRODUCT_RELATED_PRODUCT_CATEGORY(
'Linear bearing retaining cap (1)','Linear bearing retaining cap (1)',(#14799));
#14750=PRODUCT_RELATED_PRODUCT_CATEGORY(
'Linear bearing retaining cap (2)','Linear bearing retaining cap (2)',(#14800));
#14751=PRODUCT_RELATED_PRODUCT_CATEGORY(
'Linear bearing retaining cap (3)','Linear bearing retaining cap (3)',(#14801));
#14752=PRODUCT_RELATED_PRODUCT_CATEGORY(
'Linear Ball Bushing - 12 x 21 x 30 mm',
'Linear Ball Bushing - 12 x 21 x 30 mm',(#14802));
#14753=PRODUCT_RELATED_PRODUCT_CATEGORY('Steel sleeve','Steel sleeve',(#14803));
#14754=PRODUCT_RELATED_PRODUCT_CATEGORY('Ball retainer (plastic)',
'Ball retainer (plastic)',(#14804));
#14755=PRODUCT_RELATED_PRODUCT_CATEGORY('M4x10 Cap Screw',
'M4x10 Cap Screw',(#14805));
#14756=PRODUCT_RELATED_PRODUCT_CATEGORY('Cylinder foot screw',
'Cylinder foot screw',(#14806));
#14757=PRODUCT_RELATED_PRODUCT_CATEGORY('Piston rod and clevis',
'Piston rod and clevis',(#14807));
#14758=PRODUCT_RELATED_PRODUCT_CATEGORY('Twenty millimetre piston',
'Twenty millimetre piston',(#14808));
#14759=PRODUCT_RELATED_PRODUCT_CATEGORY('Piston seal','Piston seal',(#14809));
#14760=PRODUCT_RELATED_PRODUCT_CATEGORY('Piston rod','Piston rod',(#14810));
#14761=PRODUCT_RELATED_PRODUCT_CATEGORY('Cap Screw - M4x16',
'Cap Screw - M4x16',(#14811));
#14762=PRODUCT_RELATED_PRODUCT_CATEGORY('Six-millimetre-pin rod clevis',
'Six-millimetre-pin rod clevis',(#14812));
#14763=PRODUCT_RELATED_PRODUCT_CATEGORY('Socket Set Screw - M4x6',
'Socket Set Screw - M4x6',(#14813));
#14764=PRODUCT_RELATED_PRODUCT_CATEGORY('Clevis Pin - 6x30',
'Clevis Pin - 6x30',(#14814));
#14765=PRODUCT_RELATED_PRODUCT_CATEGORY('Flat Washer - M6',
'Flat Washer - M6',(#14815));
#14766=PRODUCT_RELATED_PRODUCT_CATEGORY('Split Pin - 1.6x16',
'Split Pin - 1.6x16',(#14816));
#14767=PRODUCT_RELATED_PRODUCT_CATEGORY('Stepped guide rod',
'Stepped guide rod',(#14817));
#14768=PRODUCT_RELATED_PRODUCT_CATEGORY('Stepped guide rod (1)',
'Stepped guide rod (1)',(#14818));
#14769=PRODUCT_RELATED_PRODUCT_CATEGORY('Product stop crosshead',
'Product stop crosshead',(#14819));
#14770=PRODUCT_RELATED_PRODUCT_CATEGORY('Flat Washer - M6 (1)',
'Flat Washer - M6 (1)',(#14820));
#14771=PRODUCT_RELATED_PRODUCT_CATEGORY('Hex Nut - M6','Hex Nut - M6',(#14821));
#14772=APPLICATION_PROTOCOL_DEFINITION('international standard',
'automotive_design',2009,#14773);
#14773=APPLICATION_CONTEXT(
'Core Data for Automotive Mechanical Design Process');
#14774=PRODUCT_CONTEXT('part definition',#14773,'mechanical');
#14775=PRODUCT('PAT-048','PAT-048',
'PAT-048',(#14774));
#14776=PRODUCT('Twenty millimetre bore cylinder and flow controls',
'Twenty millimetre bore cylinder and flow controls',
'Twenty millimetre bore cylinder and flow controls',(#14774));
#14777=PRODUCT('Front cylinder cap','Front cylinder cap',
'Front cylinder cap',(#14774));
#14778=PRODUCT('Needle flow-control fitting',
'Needle flow-control fitting','Needle flow-control fitting',(#14774));
#14779=PRODUCT('Metering needle and grip','Metering needle and grip',
'Metering needle and grip',(#14774));
#14780=PRODUCT('Rear cylinder cap','Rear cylinder cap',
'Rear cylinder cap',(#14774));
#14781=PRODUCT('Needle flow-control fitting (1)',
'Needle flow-control fitting (1)','Needle flow-control fitting (1)',(#14774));
#14782=PRODUCT('Metering needle and grip (1)',
'Metering needle and grip (1)','Metering needle and grip (1)',(#14774));
#14783=PRODUCT('Twenty millimetre bore barrel',
'Twenty millimetre bore barrel','Twenty millimetre bore barrel',(#14774));
#14784=PRODUCT('Barrel end gasket','Barrel end gasket',
'Barrel end gasket',(#14774));
#14785=PRODUCT('Barrel end gasket (1)','Barrel end gasket (1)',
'Barrel end gasket (1)',(#14774));
#14786=PRODUCT('Recessed cylinder mounting foot',
'Recessed cylinder mounting foot','Recessed cylinder mounting foot',(#14774));
#14787=PRODUCT('Cap Screw - M5x20','Cap Screw - M5x20',
'Cap Screw - M5x20',(#14774));
#14788=PRODUCT(
'Push-In Tube Fitting - 6 mm Tube, 1-8 Inch Tapered Pipe Thread',
'Push-In Tube Fitting - 6 mm Tube, 1-8 Inch Tapered Pipe Thread',
'Push-In Tube Fitting - 6 mm Tube, 1-8 Inch Tapered Pipe Thread',(#14774));
#14789=PRODUCT('Body','Body','Body',(#14774));
#14790=PRODUCT('Release collar','Release collar','Release collar',(#14774));
#14791=PRODUCT('O-Ring','O-Ring','O-Ring',(#14774));
#14792=PRODUCT('Rod guide','Rod guide','Rod guide',(#14774));
#14793=PRODUCT('Rod seal','Rod seal','Rod seal',(#14774));
#14794=PRODUCT('M5 tie rod','M5 tie rod','M5 tie rod',(#14774));
#14795=PRODUCT('Flat Washer - M5','Flat Washer - M5','Flat Washer - M5',
(#14774));
#14796=PRODUCT('Hex Nut - M5','Hex Nut - M5','Hex Nut - M5',(#14774));
#14797=PRODUCT('Cylinder and guide mounting frame',
'Cylinder and guide mounting frame','Cylinder and guide mounting frame',
(#14774));
#14798=PRODUCT('Linear bearing retaining cap',
'Linear bearing retaining cap','Linear bearing retaining cap',(#14774));
#14799=PRODUCT('Linear bearing retaining cap (1)',
'Linear bearing retaining cap (1)','Linear bearing retaining cap (1)',(#14774));
#14800=PRODUCT('Linear bearing retaining cap (2)',
'Linear bearing retaining cap (2)','Linear bearing retaining cap (2)',(#14774));
#14801=PRODUCT('Linear bearing retaining cap (3)',
'Linear bearing retaining cap (3)','Linear bearing retaining cap (3)',(#14774));
#14802=PRODUCT('Linear Ball Bushing - 12 x 21 x 30 mm',
'Linear Ball Bushing - 12 x 21 x 30 mm',
'Linear Ball Bushing - 12 x 21 x 30 mm',(#14774));
#14803=PRODUCT('Steel sleeve','Steel sleeve','Steel sleeve',(#14774));
#14804=PRODUCT('Ball retainer (plastic)','Ball retainer (plastic)',
'Ball retainer (plastic)',(#14774));
#14805=PRODUCT('M4x10 Cap Screw','M4x10 Cap Screw','M4x10 Cap Screw',(#14774));
#14806=PRODUCT('Cylinder foot screw','Cylinder foot screw',
'Cylinder foot screw',(#14774));
#14807=PRODUCT('Piston rod and clevis','Piston rod and clevis',
'Piston rod and clevis',(#14774));
#14808=PRODUCT('Twenty millimetre piston','Twenty millimetre piston',
'Twenty millimetre piston',(#14774));
#14809=PRODUCT('Piston seal','Piston seal','Piston seal',(#14774));
#14810=PRODUCT('Piston rod','Piston rod','Piston rod',(#14774));
#14811=PRODUCT('Cap Screw - M4x16','Cap Screw - M4x16',
'Cap Screw - M4x16',(#14774));
#14812=PRODUCT('Six-millimetre-pin rod clevis',
'Six-millimetre-pin rod clevis','Six-millimetre-pin rod clevis',(#14774));
#14813=PRODUCT('Socket Set Screw - M4x6','Socket Set Screw - M4x6',
'Socket Set Screw - M4x6',(#14774));
#14814=PRODUCT('Clevis Pin - 6x30','Clevis Pin - 6x30',
'Clevis Pin - 6x30',(#14774));
#14815=PRODUCT('Flat Washer - M6','Flat Washer - M6','Flat Washer - M6',
(#14774));
#14816=PRODUCT('Split Pin - 1.6x16','Split Pin - 1.6x16',
'Split Pin - 1.6x16',(#14774));
#14817=PRODUCT('Stepped guide rod','Stepped guide rod',
'Stepped guide rod',(#14774));
#14818=PRODUCT('Stepped guide rod (1)','Stepped guide rod (1)',
'Stepped guide rod (1)',(#14774));
#14819=PRODUCT('Product stop crosshead','Product stop crosshead',
'Product stop crosshead',(#14774));
#14820=PRODUCT('Flat Washer - M6 (1)','Flat Washer - M6 (1)',
'Flat Washer - M6 (1)',(#14774));
#14821=PRODUCT('Hex Nut - M6','Hex Nut - M6','Hex Nut - M6',(#14774));
#14822=PRESENTATION_STYLE_ASSIGNMENT((#14828));
#14823=PRESENTATION_STYLE_ASSIGNMENT((#14829));
#14824=PRESENTATION_STYLE_ASSIGNMENT((#14830));
#14825=PRESENTATION_STYLE_ASSIGNMENT((#14831));
#14826=PRESENTATION_STYLE_ASSIGNMENT((#14832));
#14827=PRESENTATION_STYLE_ASSIGNMENT((#14833));
#14828=SURFACE_STYLE_USAGE(.BOTH.,#14834);
#14829=SURFACE_STYLE_USAGE(.BOTH.,#14835);
#14830=SURFACE_STYLE_USAGE(.BOTH.,#14836);
#14831=SURFACE_STYLE_USAGE(.BOTH.,#14837);
#14832=SURFACE_STYLE_USAGE(.BOTH.,#14838);
#14833=SURFACE_STYLE_USAGE(.BOTH.,#14839);
#14834=SURFACE_SIDE_STYLE('',(#14840));
#14835=SURFACE_SIDE_STYLE('',(#14841));
#14836=SURFACE_SIDE_STYLE('',(#14842));
#14837=SURFACE_SIDE_STYLE('',(#14843));
#14838=SURFACE_SIDE_STYLE('',(#14844));
#14839=SURFACE_SIDE_STYLE('',(#14845));
#14840=SURFACE_STYLE_FILL_AREA(#14846);
#14841=SURFACE_STYLE_FILL_AREA(#14847);
#14842=SURFACE_STYLE_FILL_AREA(#14848);
#14843=SURFACE_STYLE_FILL_AREA(#14849);
#14844=SURFACE_STYLE_FILL_AREA(#14850);
#14845=SURFACE_STYLE_FILL_AREA(#14851);
#14846=FILL_AREA_STYLE('Steel - Satin',(#14852));
#14847=FILL_AREA_STYLE('CAD Library Painted - Engineering blue',(#14853));
#14848=FILL_AREA_STYLE('CAD Library Painted - Graphite',(#14854));
#14849=FILL_AREA_STYLE('CAD Library Painted - Off white',(#14855));
#14850=FILL_AREA_STYLE('CAD Library Painted - Deep blue',(#14856));
#14851=FILL_AREA_STYLE('CAD Library Painted - Steel gray',(#14857));
#14852=FILL_AREA_STYLE_COLOUR('Steel - Satin',#14858);
#14853=FILL_AREA_STYLE_COLOUR('CAD Library Painted - Engineering blue',
#14859);
#14854=FILL_AREA_STYLE_COLOUR('CAD Library Painted - Graphite',#14860);
#14855=FILL_AREA_STYLE_COLOUR('CAD Library Painted - Off white',#14861);
#14856=FILL_AREA_STYLE_COLOUR('CAD Library Painted - Deep blue',#14862);
#14857=FILL_AREA_STYLE_COLOUR('CAD Library Painted - Steel gray',#14863);
#14858=COLOUR_RGB('Steel - Satin',0.627450980392157,0.627450980392157,0.627450980392157);
#14859=COLOUR_RGB('CAD Library Painted - Engineering blue',0.12156862745098,
0.356862745098039,0.6);
#14860=COLOUR_RGB('CAD Library Painted - Graphite',0.0980392156862745,0.109803921568627,
0.125490196078431);
#14861=COLOUR_RGB('CAD Library Painted - Off white',0.909803921568627,0.901960784313726,
0.858823529411765);
#14862=COLOUR_RGB('CAD Library Painted - Deep blue',0.0784313725490196,
0.203921568627451,0.349019607843137);
#14863=COLOUR_RGB('CAD Library Painted - Steel gray',0.592156862745098,
0.631372549019608,0.67843137254902);
#14864=COLOUR_RGB('Dark Blue',0.08,0.2,0.34);
#14865=FILL_AREA_STYLE_COLOUR('',#14864);
#14866=FILL_AREA_STYLE('',(#14865));
#14867=SURFACE_STYLE_FILL_AREA(#14866);
#14868=SURFACE_SIDE_STYLE('',(#14867));
#14869=SURFACE_STYLE_USAGE(.BOTH.,#14868);
#14870=PRESENTATION_STYLE_ASSIGNMENT((#14869));
#14871=COLOUR_RGB('Light Blue',0.38,0.62,0.78);
#14872=FILL_AREA_STYLE_COLOUR('',#14871);
#14873=FILL_AREA_STYLE('',(#14872));
#14874=SURFACE_STYLE_FILL_AREA(#14873);
#14875=SURFACE_SIDE_STYLE('',(#14874));
#14876=SURFACE_STYLE_USAGE(.BOTH.,#14875);
#14877=PRESENTATION_STYLE_ASSIGNMENT((#14876));
#14878=COLOUR_RGB('Sky Blue',0.24,0.69,0.87);
#14879=FILL_AREA_STYLE_COLOUR('',#14878);
#14880=FILL_AREA_STYLE('',(#14879));
#14881=SURFACE_STYLE_FILL_AREA(#14880);
#14882=SURFACE_SIDE_STYLE('',(#14881));
#14883=SURFACE_STYLE_USAGE(.BOTH.,#14882);
#14884=PRESENTATION_STYLE_ASSIGNMENT((#14883));
#14885=COLOUR_RGB('Grey',0.48,0.52,0.57);
#14886=FILL_AREA_STYLE_COLOUR('',#14885);
#14887=FILL_AREA_STYLE('',(#14886));
#14888=SURFACE_STYLE_FILL_AREA(#14887);
#14889=SURFACE_SIDE_STYLE('',(#14888));
#14890=SURFACE_STYLE_USAGE(.BOTH.,#14889);
#14891=PRESENTATION_STYLE_ASSIGNMENT((#14890));
#14892=COLOUR_RGB('Black',0.12,0.14,0.17);
#14893=FILL_AREA_STYLE_COLOUR('',#14892);
#14894=FILL_AREA_STYLE('',(#14893));
#14895=SURFACE_STYLE_FILL_AREA(#14894);
#14896=SURFACE_SIDE_STYLE('',(#14895));
#14897=SURFACE_STYLE_USAGE(.BOTH.,#14896);
#14898=PRESENTATION_STYLE_ASSIGNMENT((#14897));
#14899=COLOUR_RGB('Off White',0.89,0.88,0.83);
#14900=FILL_AREA_STYLE_COLOUR('',#14899);
#14901=FILL_AREA_STYLE('',(#14900));
#14902=SURFACE_STYLE_FILL_AREA(#14901);
#14903=SURFACE_SIDE_STYLE('',(#14902));
#14904=SURFACE_STYLE_USAGE(.BOTH.,#14903);
#14905=PRESENTATION_STYLE_ASSIGNMENT((#14904));
ENDSEC;
END-ISO-10303-21;
